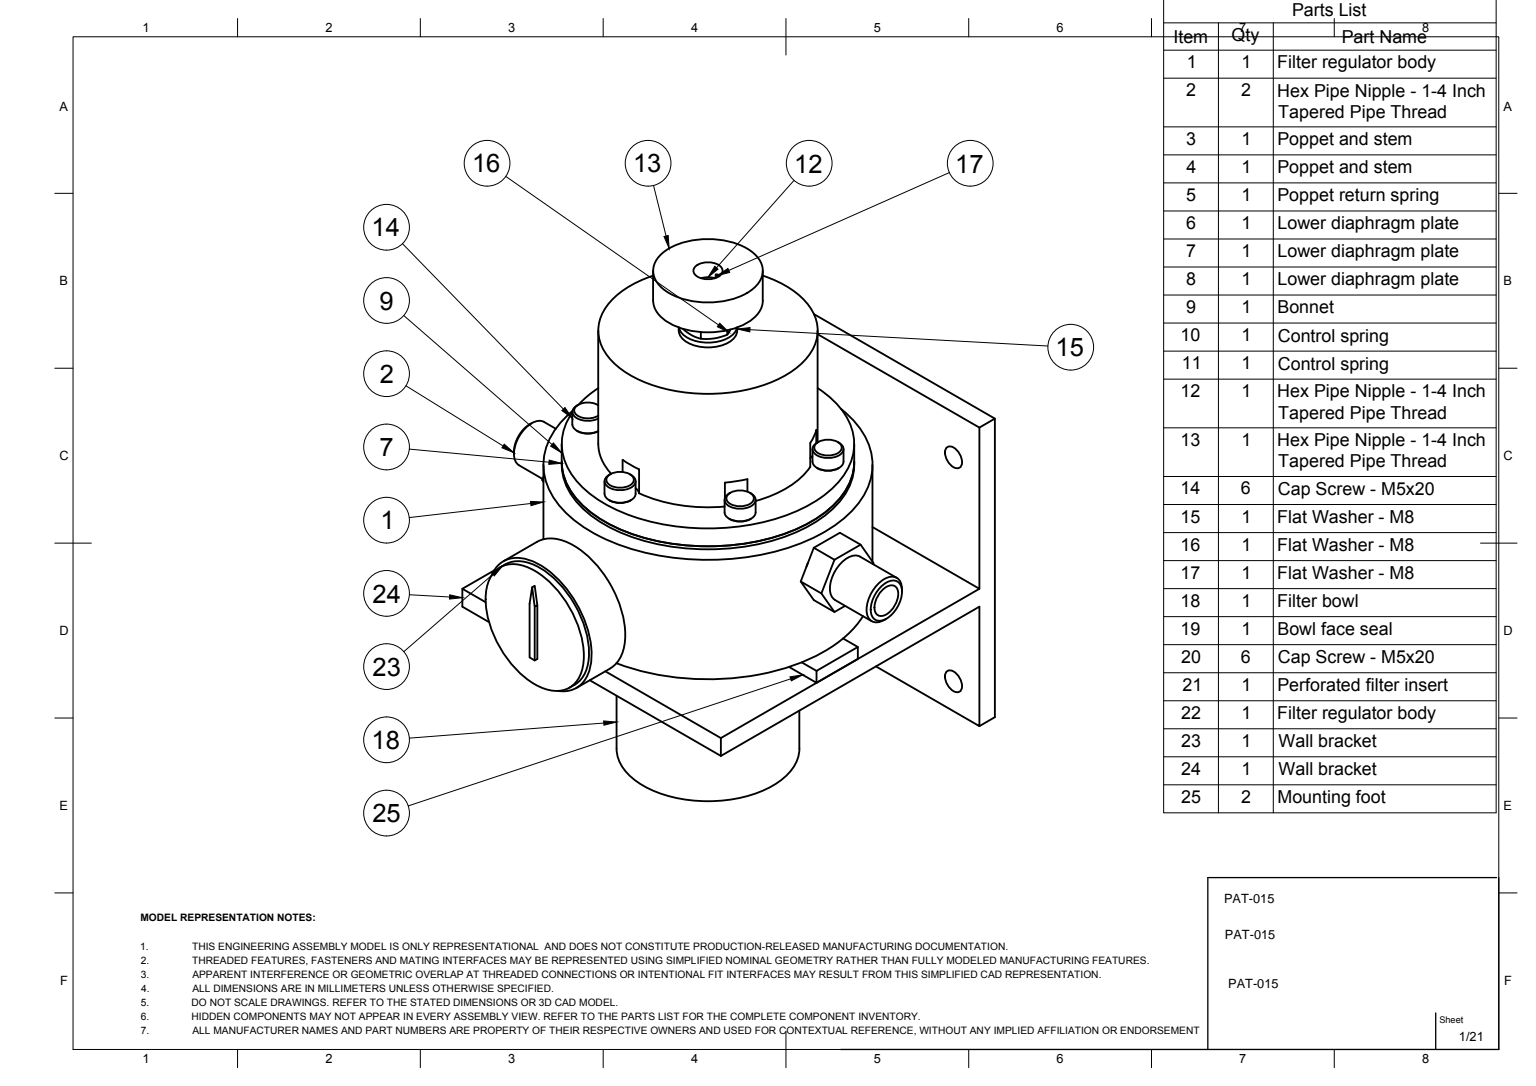
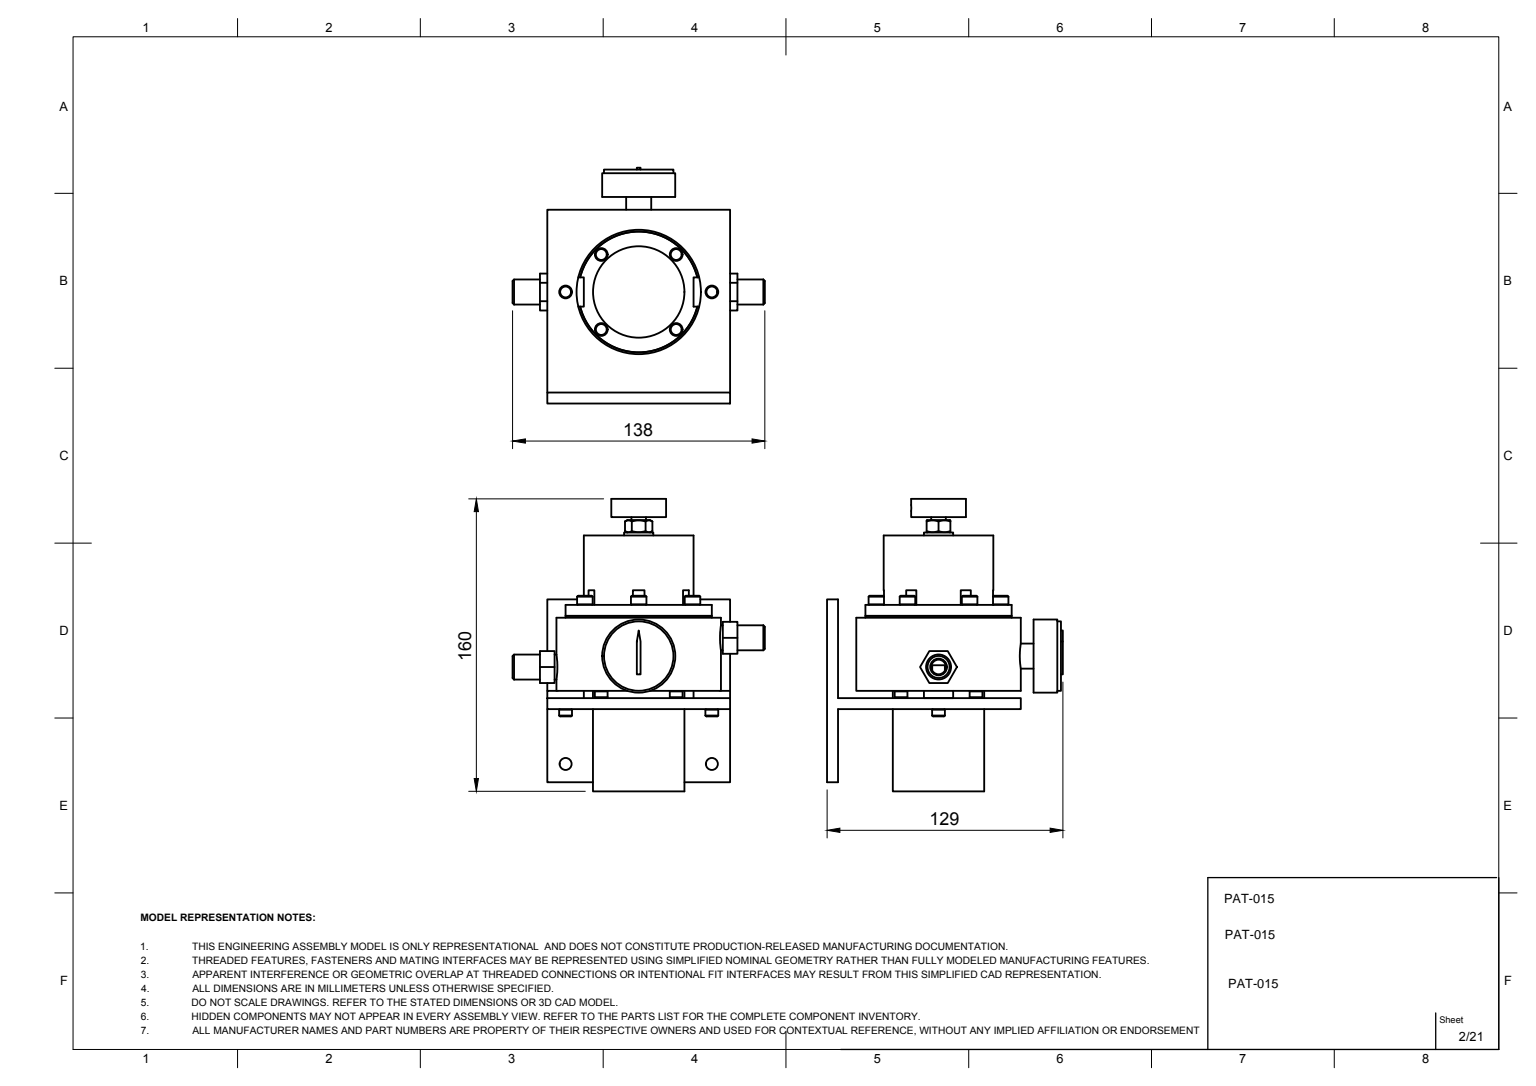
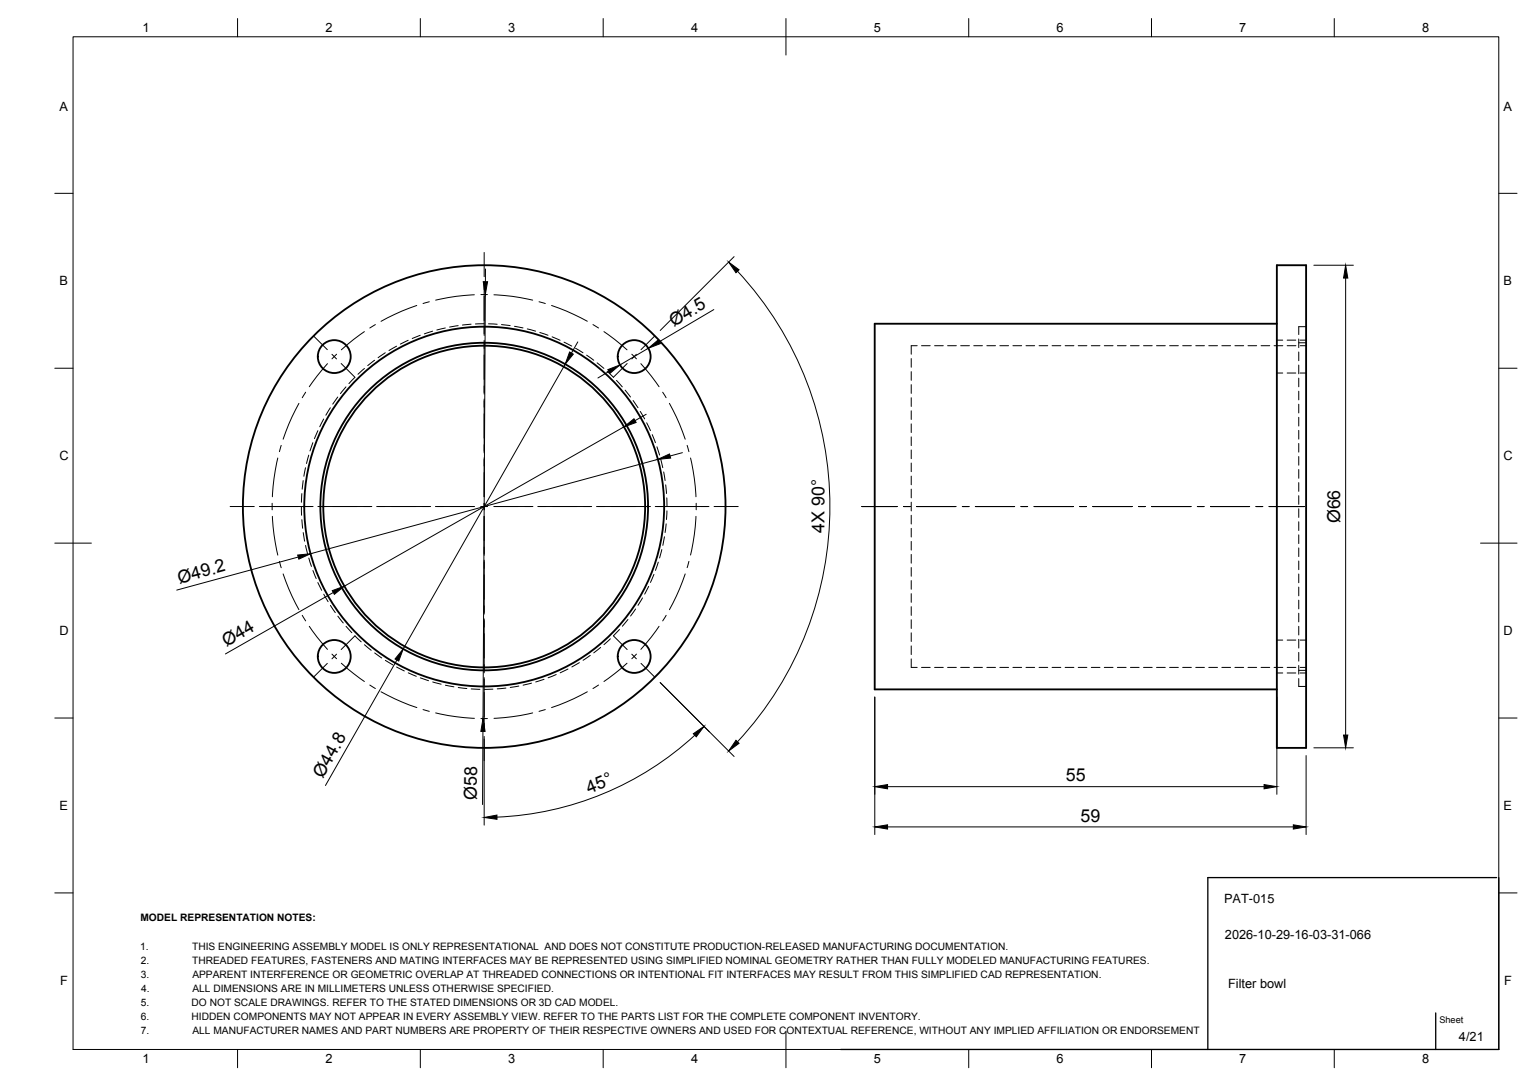
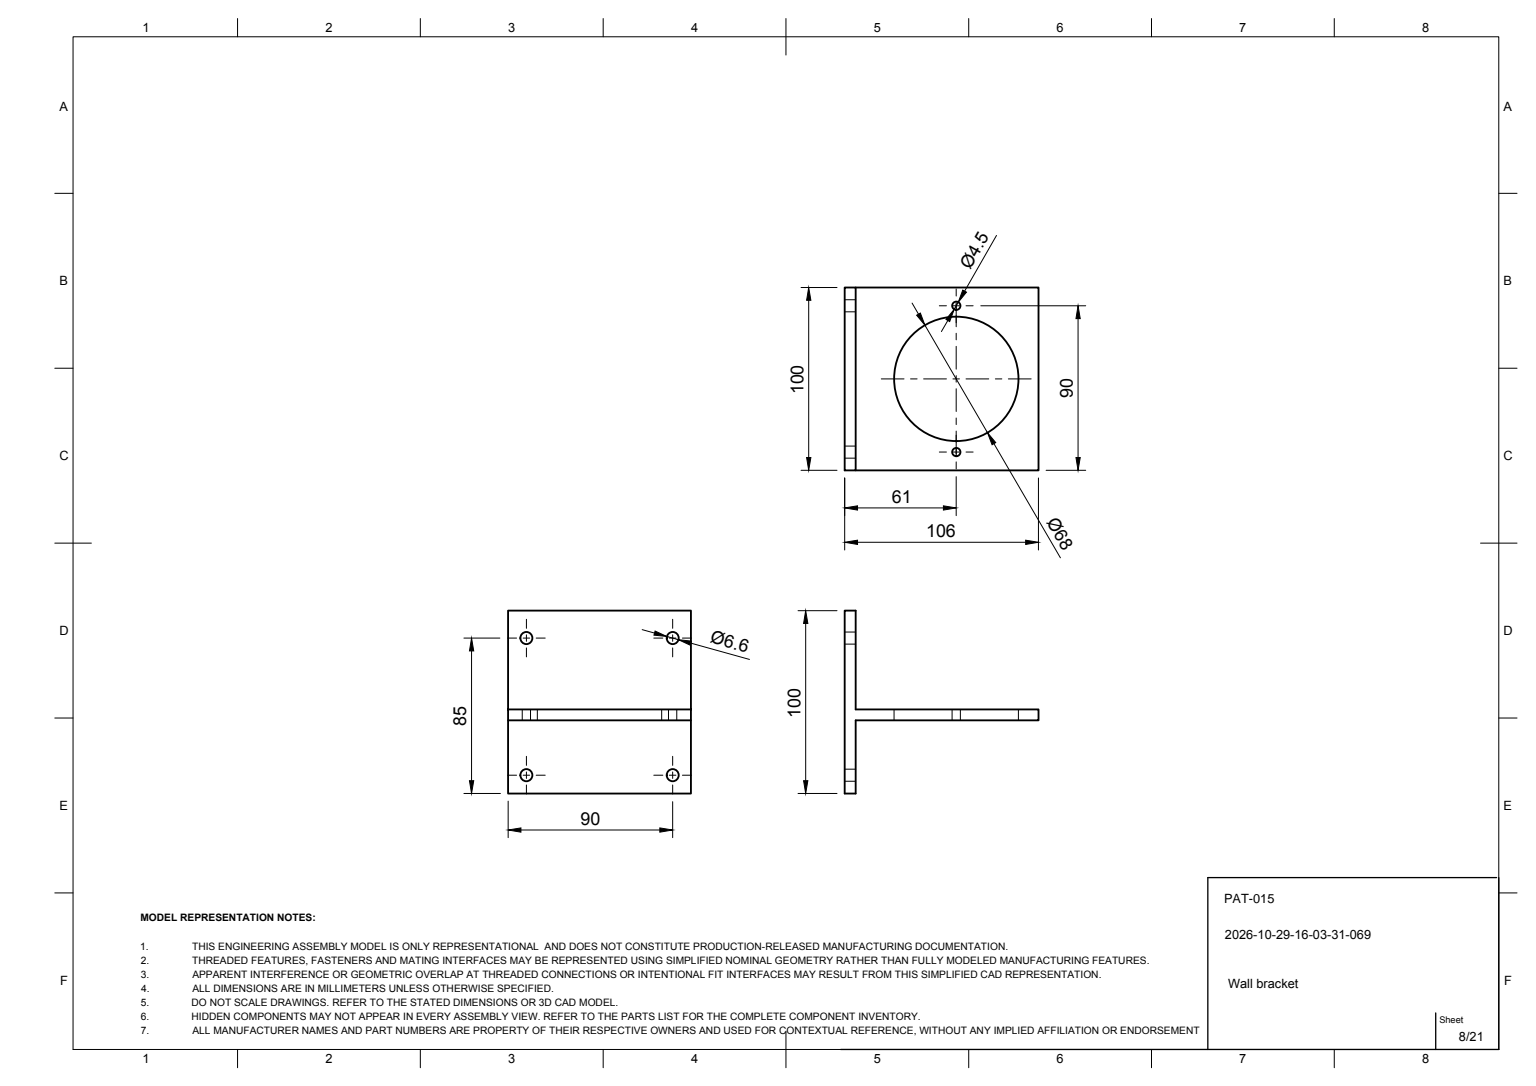
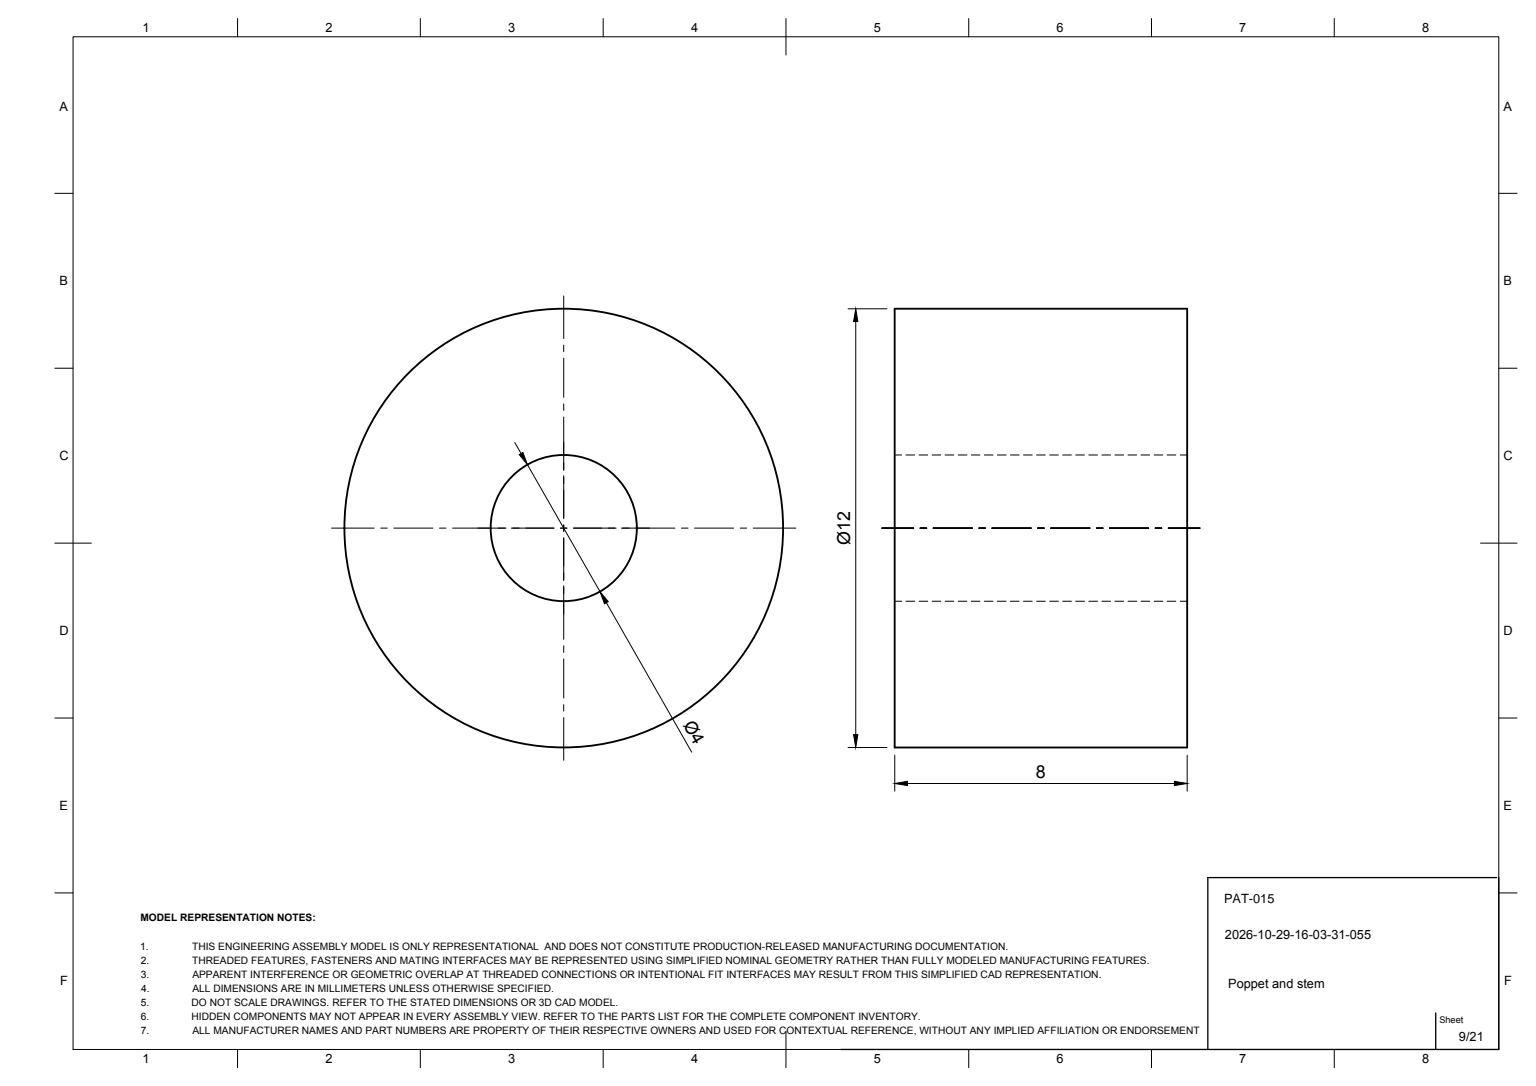
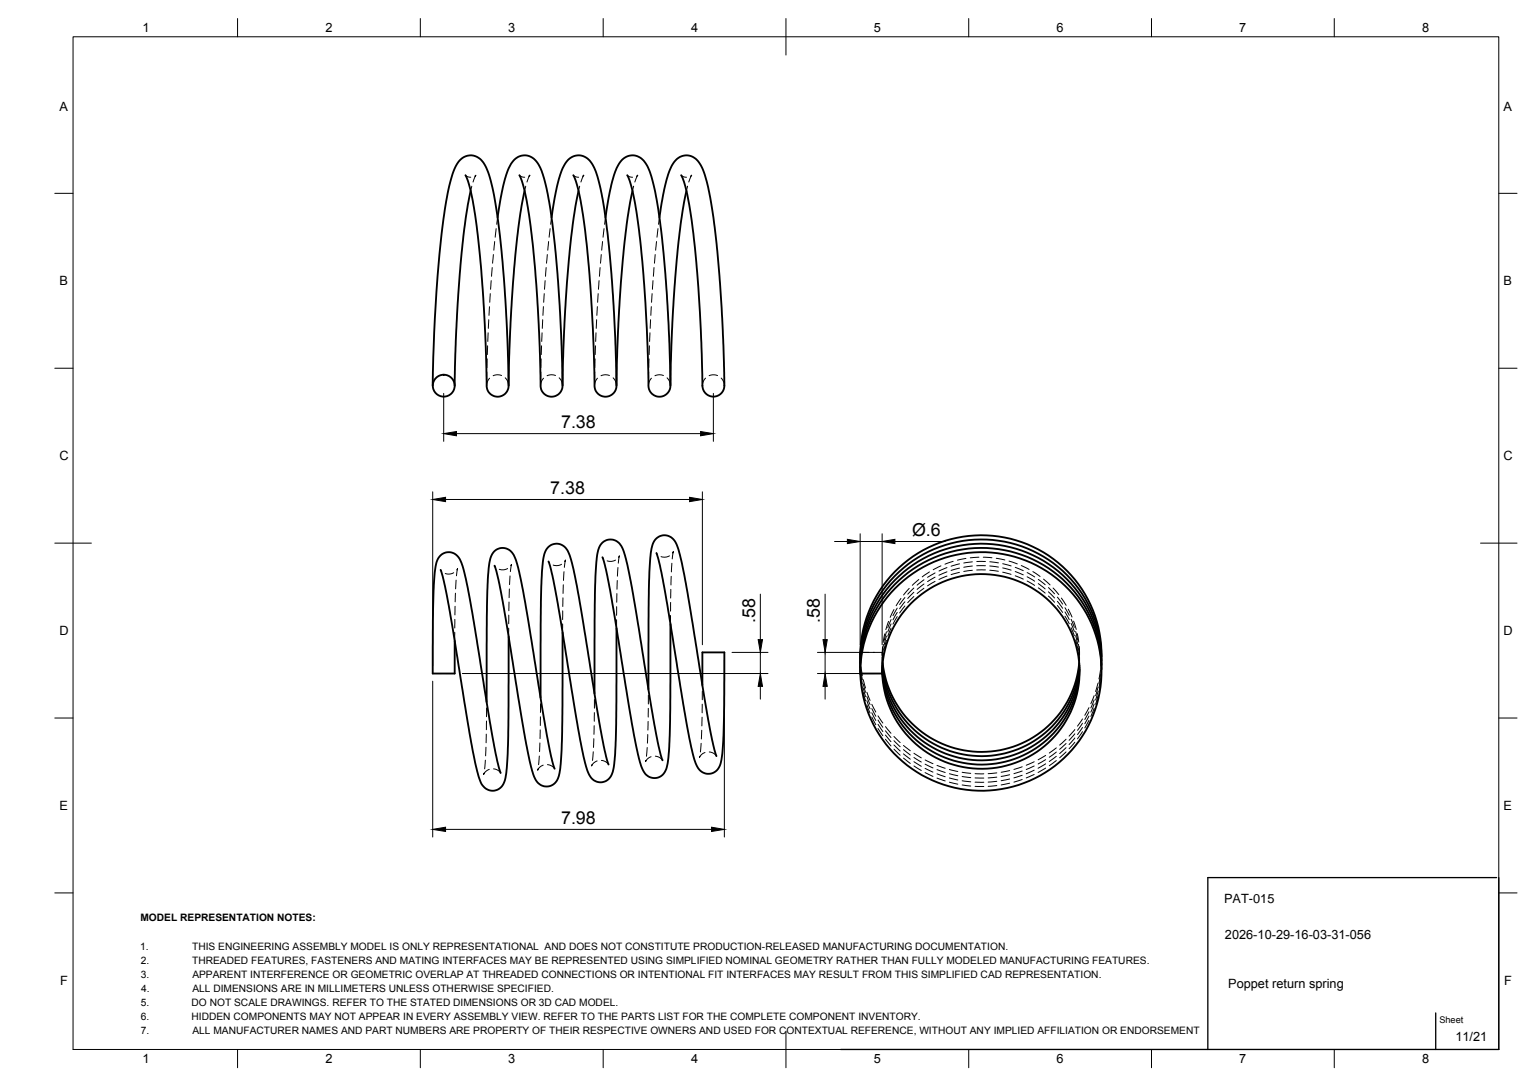
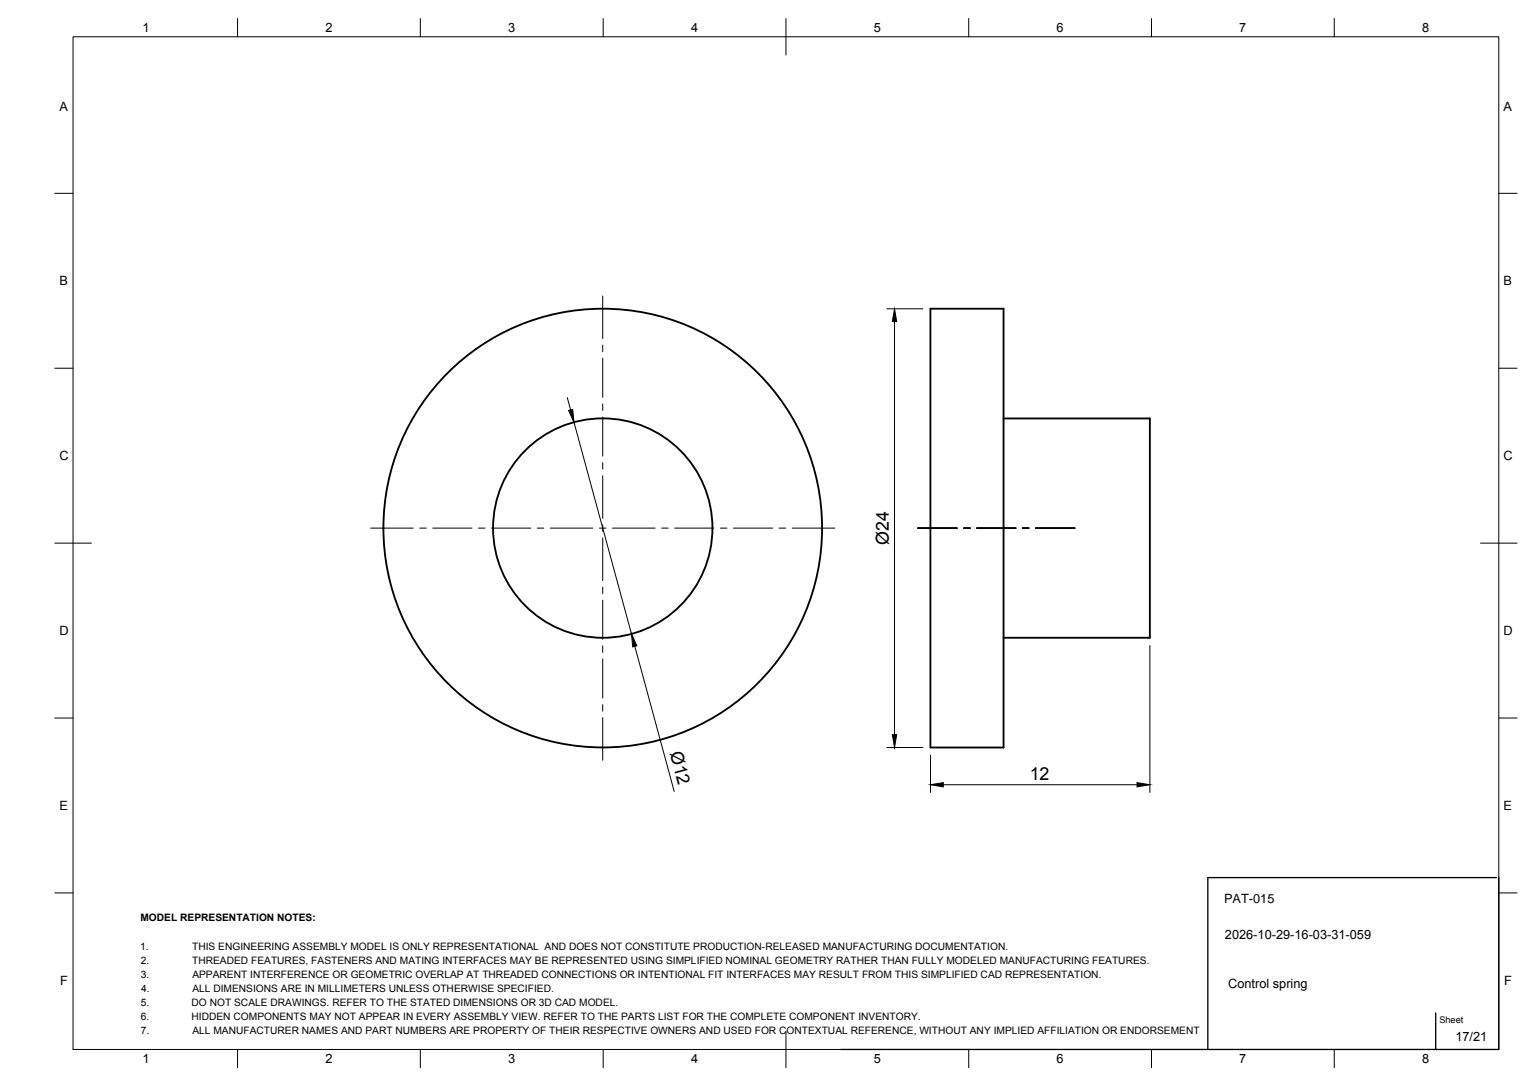
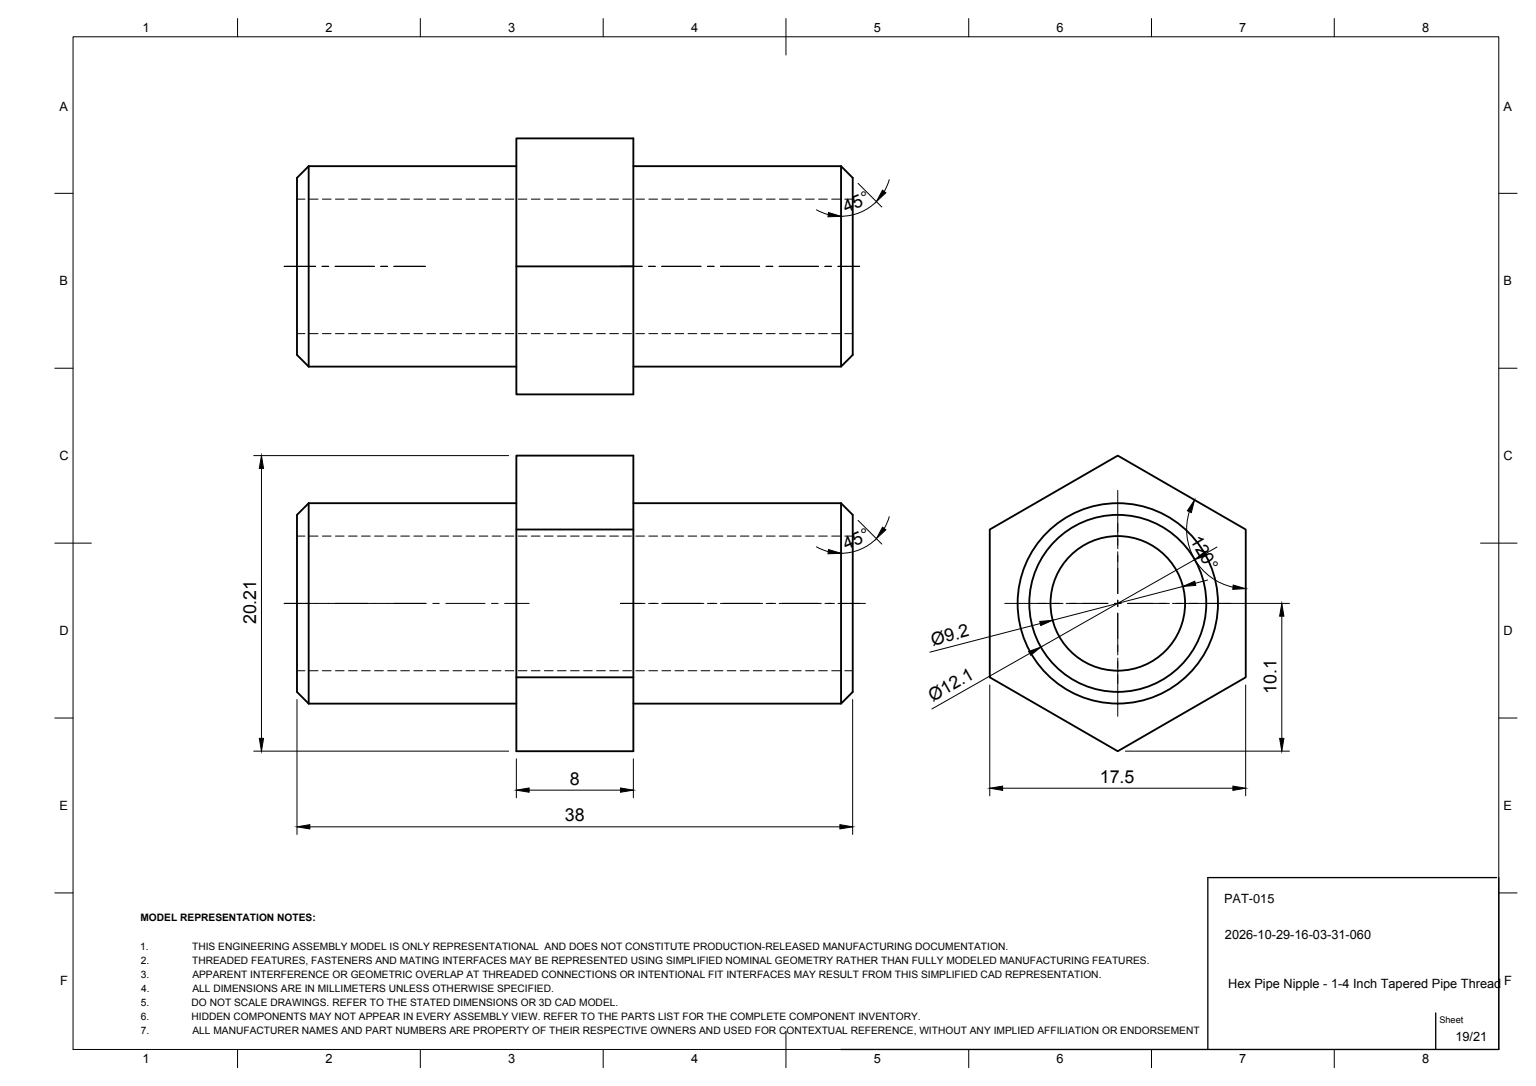
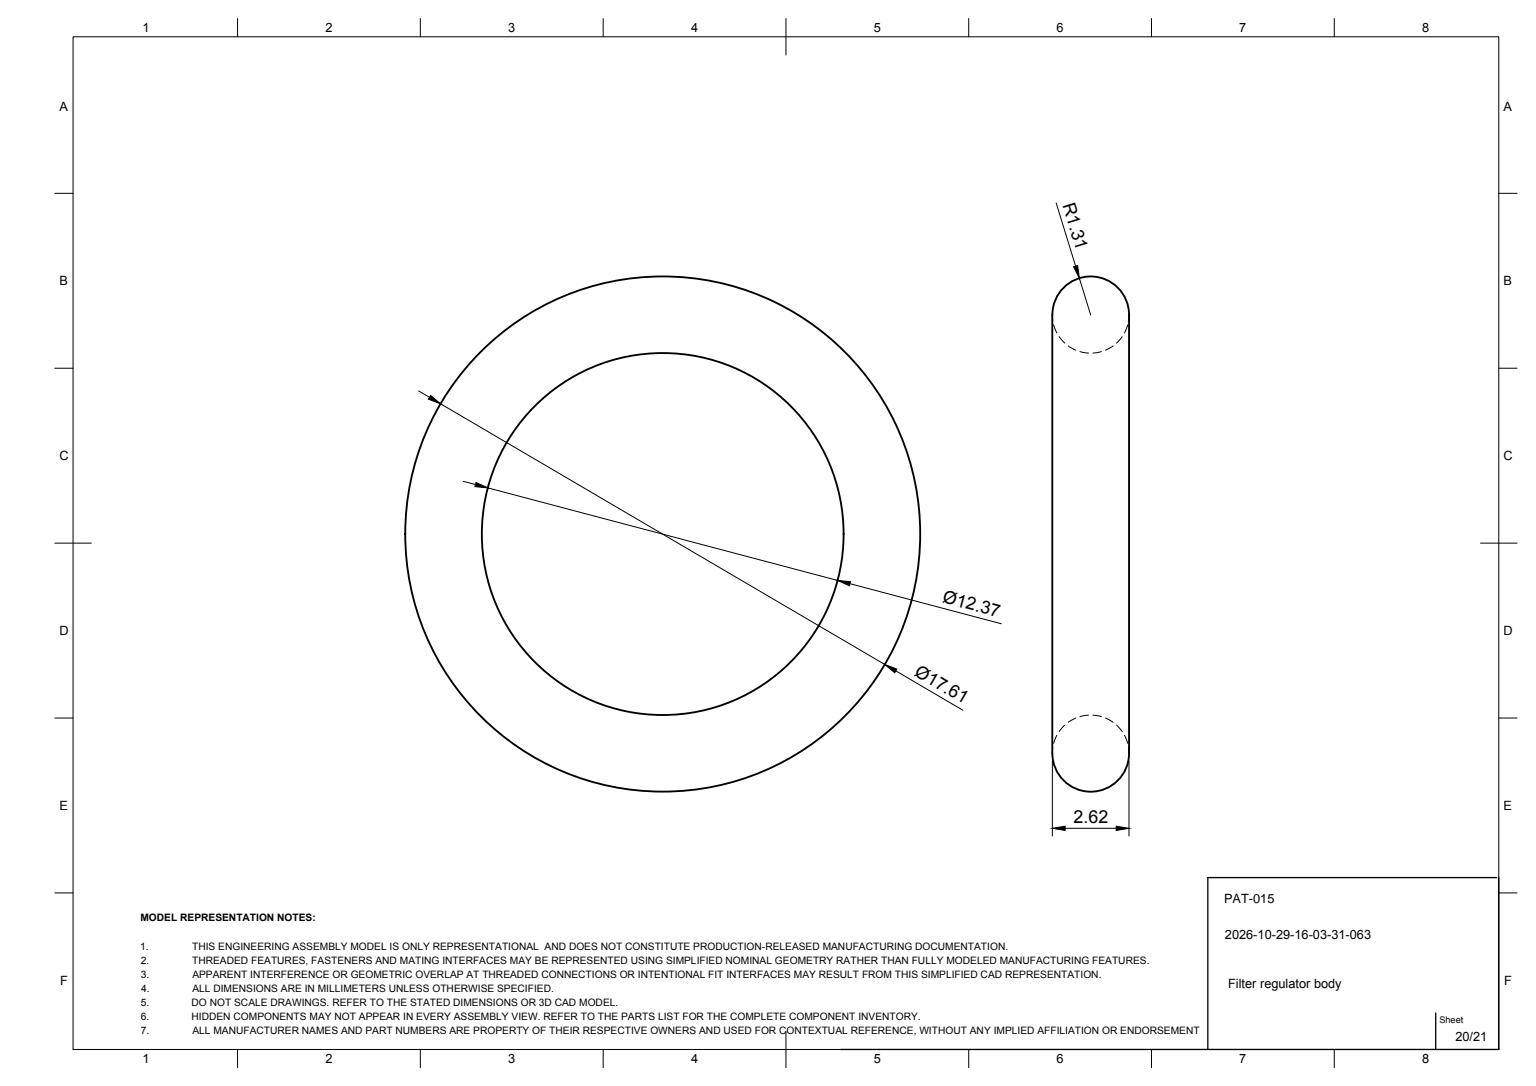
ISO-10303-21;
HEADER;
/* Generated by software containing ST-Developer
 * from STEP Tools, Inc. (www.steptools.com) 
 */

FILE_DESCRIPTION(
/* description */ ('PAT-015'),
/* implementation_level */ '2;1');

FILE_NAME(
/* name */ 'PAT-015',
/* time_stamp */ '2026-10-29T16:03:43-07:00',
/* author */ (''),
/* organization */ (''),
/* preprocessor_version */ 'ST-DEVELOPER v20.2',
/* originating_system */ 'Autodesk Translation Framework v15.17.0.0',
/* authorisation */ '');

FILE_SCHEMA (('AUTOMOTIVE_DESIGN { 1 0 10303 214 3 1 1 }'));
ENDSEC;

DATA;
#10=MECHANICAL_DESIGN_GEOMETRIC_PRESENTATION_REPRESENTATION('',(#230,#231,
#232,#233,#234,#235,#236,#237,#238,#239,#240,#241,#242,#243,#244,#245,#246,
#247,#248,#249,#250,#251,#252,#253,#254),#10266);
#11=ITEM_DEFINED_TRANSFORMATION($,$,#4971,#5521);
#12=ITEM_DEFINED_TRANSFORMATION($,$,#5114,#5522);
#13=ITEM_DEFINED_TRANSFORMATION($,$,#5118,#5523);
#14=ITEM_DEFINED_TRANSFORMATION($,$,#5144,#5524);
#15=ITEM_DEFINED_TRANSFORMATION($,$,#5166,#5525);
#16=ITEM_DEFINED_TRANSFORMATION($,$,#5198,#5526);
#17=ITEM_DEFINED_TRANSFORMATION($,$,#5198,#5527);
#18=ITEM_DEFINED_TRANSFORMATION($,$,#5222,#5528);
#19=ITEM_DEFINED_TRANSFORMATION($,$,#5231,#5529);
#20=ITEM_DEFINED_TRANSFORMATION($,$,#5253,#5530);
#21=ITEM_DEFINED_TRANSFORMATION($,$,#5262,#5531);
#22=ITEM_DEFINED_TRANSFORMATION($,$,#5289,#5532);
#23=ITEM_DEFINED_TRANSFORMATION($,$,#5306,#5533);
#24=ITEM_DEFINED_TRANSFORMATION($,$,#5377,#5534);
#25=ITEM_DEFINED_TRANSFORMATION($,$,#5382,#5535);
#26=ITEM_DEFINED_TRANSFORMATION($,$,#5392,#5536);
#27=ITEM_DEFINED_TRANSFORMATION($,$,#5398,#5537);
#28=ITEM_DEFINED_TRANSFORMATION($,$,#5413,#5538);
#29=ITEM_DEFINED_TRANSFORMATION($,$,#5413,#5539);
#30=ITEM_DEFINED_TRANSFORMATION($,$,#5413,#5540);
#31=ITEM_DEFINED_TRANSFORMATION($,$,#5413,#5541);
#32=ITEM_DEFINED_TRANSFORMATION($,$,#5413,#5542);
#33=ITEM_DEFINED_TRANSFORMATION($,$,#5413,#5543);
#34=ITEM_DEFINED_TRANSFORMATION($,$,#5439,#5544);
#35=ITEM_DEFINED_TRANSFORMATION($,$,#5448,#5545);
#36=ITEM_DEFINED_TRANSFORMATION($,$,#5464,#5546);
#37=ITEM_DEFINED_TRANSFORMATION($,$,#5495,#5547);
#38=ITEM_DEFINED_TRANSFORMATION($,$,#5495,#5548);
#39=ITEM_DEFINED_TRANSFORMATION($,$,#5495,#5549);
#40=ITEM_DEFINED_TRANSFORMATION($,$,#5495,#5550);
#41=ITEM_DEFINED_TRANSFORMATION($,$,#5481,#5551);
#42=ITEM_DEFINED_TRANSFORMATION($,$,#5485,#5552);
#43=ITEM_DEFINED_TRANSFORMATION($,$,#5495,#5553);
#44=ITEM_DEFINED_TRANSFORMATION($,$,#5485,#5554);
#45=ITEM_DEFINED_TRANSFORMATION($,$,#5495,#5555);
#46=(
REPRESENTATION_RELATIONSHIP($,$,#10355,#10354)
REPRESENTATION_RELATIONSHIP_WITH_TRANSFORMATION(#11)
SHAPE_REPRESENTATION_RELATIONSHIP()
);
#47=(
REPRESENTATION_RELATIONSHIP($,$,#10356,#10354)
REPRESENTATION_RELATIONSHIP_WITH_TRANSFORMATION(#12)
SHAPE_REPRESENTATION_RELATIONSHIP()
);
#48=(
REPRESENTATION_RELATIONSHIP($,$,#10357,#10354)
REPRESENTATION_RELATIONSHIP_WITH_TRANSFORMATION(#13)
SHAPE_REPRESENTATION_RELATIONSHIP()
);
#49=(
REPRESENTATION_RELATIONSHIP($,$,#10358,#10354)
REPRESENTATION_RELATIONSHIP_WITH_TRANSFORMATION(#14)
SHAPE_REPRESENTATION_RELATIONSHIP()
);
#50=(
REPRESENTATION_RELATIONSHIP($,$,#10359,#10354)
REPRESENTATION_RELATIONSHIP_WITH_TRANSFORMATION(#15)
SHAPE_REPRESENTATION_RELATIONSHIP()
);
#51=(
REPRESENTATION_RELATIONSHIP($,$,#10360,#10354)
REPRESENTATION_RELATIONSHIP_WITH_TRANSFORMATION(#16)
SHAPE_REPRESENTATION_RELATIONSHIP()
);
#52=(
REPRESENTATION_RELATIONSHIP($,$,#10360,#10354)
REPRESENTATION_RELATIONSHIP_WITH_TRANSFORMATION(#17)
SHAPE_REPRESENTATION_RELATIONSHIP()
);
#53=(
REPRESENTATION_RELATIONSHIP($,$,#10361,#10354)
REPRESENTATION_RELATIONSHIP_WITH_TRANSFORMATION(#18)
SHAPE_REPRESENTATION_RELATIONSHIP()
);
#54=(
REPRESENTATION_RELATIONSHIP($,$,#10362,#10354)
REPRESENTATION_RELATIONSHIP_WITH_TRANSFORMATION(#19)
SHAPE_REPRESENTATION_RELATIONSHIP()
);
#55=(
REPRESENTATION_RELATIONSHIP($,$,#10363,#10354)
REPRESENTATION_RELATIONSHIP_WITH_TRANSFORMATION(#20)
SHAPE_REPRESENTATION_RELATIONSHIP()
);
#56=(
REPRESENTATION_RELATIONSHIP($,$,#10364,#10354)
REPRESENTATION_RELATIONSHIP_WITH_TRANSFORMATION(#21)
SHAPE_REPRESENTATION_RELATIONSHIP()
);
#57=(
REPRESENTATION_RELATIONSHIP($,$,#10365,#10354)
REPRESENTATION_RELATIONSHIP_WITH_TRANSFORMATION(#22)
SHAPE_REPRESENTATION_RELATIONSHIP()
);
#58=(
REPRESENTATION_RELATIONSHIP($,$,#10366,#10354)
REPRESENTATION_RELATIONSHIP_WITH_TRANSFORMATION(#23)
SHAPE_REPRESENTATION_RELATIONSHIP()
);
#59=(
REPRESENTATION_RELATIONSHIP($,$,#10367,#10354)
REPRESENTATION_RELATIONSHIP_WITH_TRANSFORMATION(#24)
SHAPE_REPRESENTATION_RELATIONSHIP()
);
#60=(
REPRESENTATION_RELATIONSHIP($,$,#10368,#10354)
REPRESENTATION_RELATIONSHIP_WITH_TRANSFORMATION(#25)
SHAPE_REPRESENTATION_RELATIONSHIP()
);
#61=(
REPRESENTATION_RELATIONSHIP($,$,#10369,#10354)
REPRESENTATION_RELATIONSHIP_WITH_TRANSFORMATION(#26)
SHAPE_REPRESENTATION_RELATIONSHIP()
);
#62=(
REPRESENTATION_RELATIONSHIP($,$,#10370,#10354)
REPRESENTATION_RELATIONSHIP_WITH_TRANSFORMATION(#27)
SHAPE_REPRESENTATION_RELATIONSHIP()
);
#63=(
REPRESENTATION_RELATIONSHIP($,$,#10371,#10354)
REPRESENTATION_RELATIONSHIP_WITH_TRANSFORMATION(#28)
SHAPE_REPRESENTATION_RELATIONSHIP()
);
#64=(
REPRESENTATION_RELATIONSHIP($,$,#10371,#10354)
REPRESENTATION_RELATIONSHIP_WITH_TRANSFORMATION(#29)
SHAPE_REPRESENTATION_RELATIONSHIP()
);
#65=(
REPRESENTATION_RELATIONSHIP($,$,#10371,#10354)
REPRESENTATION_RELATIONSHIP_WITH_TRANSFORMATION(#30)
SHAPE_REPRESENTATION_RELATIONSHIP()
);
#66=(
REPRESENTATION_RELATIONSHIP($,$,#10371,#10354)
REPRESENTATION_RELATIONSHIP_WITH_TRANSFORMATION(#31)
SHAPE_REPRESENTATION_RELATIONSHIP()
);
#67=(
REPRESENTATION_RELATIONSHIP($,$,#10371,#10354)
REPRESENTATION_RELATIONSHIP_WITH_TRANSFORMATION(#32)
SHAPE_REPRESENTATION_RELATIONSHIP()
);
#68=(
REPRESENTATION_RELATIONSHIP($,$,#10371,#10354)
REPRESENTATION_RELATIONSHIP_WITH_TRANSFORMATION(#33)
SHAPE_REPRESENTATION_RELATIONSHIP()
);
#69=(
REPRESENTATION_RELATIONSHIP($,$,#10372,#10354)
REPRESENTATION_RELATIONSHIP_WITH_TRANSFORMATION(#34)
SHAPE_REPRESENTATION_RELATIONSHIP()
);
#70=(
REPRESENTATION_RELATIONSHIP($,$,#10373,#10354)
REPRESENTATION_RELATIONSHIP_WITH_TRANSFORMATION(#35)
SHAPE_REPRESENTATION_RELATIONSHIP()
);
#71=(
REPRESENTATION_RELATIONSHIP($,$,#10374,#10354)
REPRESENTATION_RELATIONSHIP_WITH_TRANSFORMATION(#36)
SHAPE_REPRESENTATION_RELATIONSHIP()
);
#72=(
REPRESENTATION_RELATIONSHIP($,$,#10377,#10354)
REPRESENTATION_RELATIONSHIP_WITH_TRANSFORMATION(#37)
SHAPE_REPRESENTATION_RELATIONSHIP()
);
#73=(
REPRESENTATION_RELATIONSHIP($,$,#10377,#10354)
REPRESENTATION_RELATIONSHIP_WITH_TRANSFORMATION(#38)
SHAPE_REPRESENTATION_RELATIONSHIP()
);
#74=(
REPRESENTATION_RELATIONSHIP($,$,#10377,#10354)
REPRESENTATION_RELATIONSHIP_WITH_TRANSFORMATION(#39)
SHAPE_REPRESENTATION_RELATIONSHIP()
);
#75=(
REPRESENTATION_RELATIONSHIP($,$,#10377,#10354)
REPRESENTATION_RELATIONSHIP_WITH_TRANSFORMATION(#40)
SHAPE_REPRESENTATION_RELATIONSHIP()
);
#76=(
REPRESENTATION_RELATIONSHIP($,$,#10375,#10354)
REPRESENTATION_RELATIONSHIP_WITH_TRANSFORMATION(#41)
SHAPE_REPRESENTATION_RELATIONSHIP()
);
#77=(
REPRESENTATION_RELATIONSHIP($,$,#10376,#10354)
REPRESENTATION_RELATIONSHIP_WITH_TRANSFORMATION(#42)
SHAPE_REPRESENTATION_RELATIONSHIP()
);
#78=(
REPRESENTATION_RELATIONSHIP($,$,#10377,#10354)
REPRESENTATION_RELATIONSHIP_WITH_TRANSFORMATION(#43)
SHAPE_REPRESENTATION_RELATIONSHIP()
);
#79=(
REPRESENTATION_RELATIONSHIP($,$,#10376,#10354)
REPRESENTATION_RELATIONSHIP_WITH_TRANSFORMATION(#44)
SHAPE_REPRESENTATION_RELATIONSHIP()
);
#80=(
REPRESENTATION_RELATIONSHIP($,$,#10377,#10354)
REPRESENTATION_RELATIONSHIP_WITH_TRANSFORMATION(#45)
SHAPE_REPRESENTATION_RELATIONSHIP()
);
#81=CONTEXT_DEPENDENT_SHAPE_REPRESENTATION(#46,#10319);
#82=CONTEXT_DEPENDENT_SHAPE_REPRESENTATION(#47,#10320);
#83=CONTEXT_DEPENDENT_SHAPE_REPRESENTATION(#48,#10321);
#84=CONTEXT_DEPENDENT_SHAPE_REPRESENTATION(#49,#10322);
#85=CONTEXT_DEPENDENT_SHAPE_REPRESENTATION(#50,#10323);
#86=CONTEXT_DEPENDENT_SHAPE_REPRESENTATION(#51,#10324);
#87=CONTEXT_DEPENDENT_SHAPE_REPRESENTATION(#52,#10325);
#88=CONTEXT_DEPENDENT_SHAPE_REPRESENTATION(#53,#10326);
#89=CONTEXT_DEPENDENT_SHAPE_REPRESENTATION(#54,#10327);
#90=CONTEXT_DEPENDENT_SHAPE_REPRESENTATION(#55,#10328);
#91=CONTEXT_DEPENDENT_SHAPE_REPRESENTATION(#56,#10329);
#92=CONTEXT_DEPENDENT_SHAPE_REPRESENTATION(#57,#10330);
#93=CONTEXT_DEPENDENT_SHAPE_REPRESENTATION(#58,#10331);
#94=CONTEXT_DEPENDENT_SHAPE_REPRESENTATION(#59,#10332);
#95=CONTEXT_DEPENDENT_SHAPE_REPRESENTATION(#60,#10333);
#96=CONTEXT_DEPENDENT_SHAPE_REPRESENTATION(#61,#10334);
#97=CONTEXT_DEPENDENT_SHAPE_REPRESENTATION(#62,#10335);
#98=CONTEXT_DEPENDENT_SHAPE_REPRESENTATION(#63,#10336);
#99=CONTEXT_DEPENDENT_SHAPE_REPRESENTATION(#64,#10337);
#100=CONTEXT_DEPENDENT_SHAPE_REPRESENTATION(#65,#10338);
#101=CONTEXT_DEPENDENT_SHAPE_REPRESENTATION(#66,#10339);
#102=CONTEXT_DEPENDENT_SHAPE_REPRESENTATION(#67,#10340);
#103=CONTEXT_DEPENDENT_SHAPE_REPRESENTATION(#68,#10341);
#104=CONTEXT_DEPENDENT_SHAPE_REPRESENTATION(#69,#10342);
#105=CONTEXT_DEPENDENT_SHAPE_REPRESENTATION(#70,#10343);
#106=CONTEXT_DEPENDENT_SHAPE_REPRESENTATION(#71,#10344);
#107=CONTEXT_DEPENDENT_SHAPE_REPRESENTATION(#72,#10345);
#108=CONTEXT_DEPENDENT_SHAPE_REPRESENTATION(#73,#10346);
#109=CONTEXT_DEPENDENT_SHAPE_REPRESENTATION(#74,#10347);
#110=CONTEXT_DEPENDENT_SHAPE_REPRESENTATION(#75,#10348);
#111=CONTEXT_DEPENDENT_SHAPE_REPRESENTATION(#76,#10349);
#112=CONTEXT_DEPENDENT_SHAPE_REPRESENTATION(#77,#10350);
#113=CONTEXT_DEPENDENT_SHAPE_REPRESENTATION(#78,#10351);
#114=CONTEXT_DEPENDENT_SHAPE_REPRESENTATION(#79,#10352);
#115=CONTEXT_DEPENDENT_SHAPE_REPRESENTATION(#80,#10353);
#116=NEXT_ASSEMBLY_USAGE_OCCURRENCE('Filter regulator body:1',
'Filter regulator body:1','Filter regulator body:1',#10379,#10380,
'Filter regulator body:1');
#117=NEXT_ASSEMBLY_USAGE_OCCURRENCE('Bowl face seal:1',
'Bowl face seal:1','Bowl face seal:1',#10379,#10381,'Bowl face seal:1');
#118=NEXT_ASSEMBLY_USAGE_OCCURRENCE('Perforated filter insert:1',
'Perforated filter insert:1','Perforated filter insert:1',#10379,#10382,
'Perforated filter insert:1');
#119=NEXT_ASSEMBLY_USAGE_OCCURRENCE('Gauge dummy:1','Gauge dummy:1',
'Gauge dummy:1',#10379,#10383,'Gauge dummy:1');
#120=NEXT_ASSEMBLY_USAGE_OCCURRENCE('Wall bracket:1','Wall bracket:1',
'Wall bracket:1',#10379,#10384,'Wall bracket:1');
#121=NEXT_ASSEMBLY_USAGE_OCCURRENCE(
'Hex Pipe Nipple - 1-4 Inch Tapered Pipe Thread:1',
'Hex Pipe Nipple - 1-4 Inch Tapered Pipe Thread:1',
'Hex Pipe Nipple - 1-4 Inch Tapered Pipe Thread:1',#10379,#10385,
'Hex Pipe Nipple - 1-4 Inch Tapered Pipe Thread:1');
#122=NEXT_ASSEMBLY_USAGE_OCCURRENCE(
'Hex Pipe Nipple - 1-4 Inch Tapered Pipe Thread:2',
'Hex Pipe Nipple - 1-4 Inch Tapered Pipe Thread:2',
'Hex Pipe Nipple - 1-4 Inch Tapered Pipe Thread:2',#10379,#10385,
'Hex Pipe Nipple - 1-4 Inch Tapered Pipe Thread:2');
#123=NEXT_ASSEMBLY_USAGE_OCCURRENCE('Valve seat:1','Valve seat:1',
'Valve seat:1',#10379,#10386,'Valve seat:1');
#124=NEXT_ASSEMBLY_USAGE_OCCURRENCE('Poppet and stem:1',
'Poppet and stem:1','Poppet and stem:1',#10379,#10387,
'Poppet and stem:1');
#125=NEXT_ASSEMBLY_USAGE_OCCURRENCE('Lower diaphragm plate:1',
'Lower diaphragm plate:1','Lower diaphragm plate:1',#10379,#10388,
'Lower diaphragm plate:1');
#126=NEXT_ASSEMBLY_USAGE_OCCURRENCE('Diaphragm:1','Diaphragm:1',
'Diaphragm:1',#10379,#10389,'Diaphragm:1');
#127=NEXT_ASSEMBLY_USAGE_OCCURRENCE('Upper diaphragm plate:1',
'Upper diaphragm plate:1','Upper diaphragm plate:1',#10379,#10390,
'Upper diaphragm plate:1');
#128=NEXT_ASSEMBLY_USAGE_OCCURRENCE('Bonnet:1','Bonnet:1','Bonnet:1',#10379,
#10391,'Bonnet:1');
#129=NEXT_ASSEMBLY_USAGE_OCCURRENCE('Control spring:1',
'Control spring:1','Control spring:1',#10379,#10392,'Control spring:1');
#130=NEXT_ASSEMBLY_USAGE_OCCURRENCE('Adjuster spring shoe:1',
'Adjuster spring shoe:1','Adjuster spring shoe:1',#10379,#10393,
'Adjuster spring shoe:1');
#131=NEXT_ASSEMBLY_USAGE_OCCURRENCE('Adjusting screw:1',
'Adjusting screw:1','Adjusting screw:1',#10379,#10394,
'Adjusting screw:1');
#132=NEXT_ASSEMBLY_USAGE_OCCURRENCE('Adjuster knob:1','Adjuster knob:1',
'Adjuster knob:1',#10379,#10395,'Adjuster knob:1');
#133=NEXT_ASSEMBLY_USAGE_OCCURRENCE('Cap Screw - M5x20:1',
'Cap Screw - M5x20:1','Cap Screw - M5x20:1',#10379,#10396,
'Cap Screw - M5x20:1');
#134=NEXT_ASSEMBLY_USAGE_OCCURRENCE('Cap Screw - M5x20:2',
'Cap Screw - M5x20:2','Cap Screw - M5x20:2',#10379,#10396,
'Cap Screw - M5x20:2');
#135=NEXT_ASSEMBLY_USAGE_OCCURRENCE('Cap Screw - M5x20:3',
'Cap Screw - M5x20:3','Cap Screw - M5x20:3',#10379,#10396,
'Cap Screw - M5x20:3');
#136=NEXT_ASSEMBLY_USAGE_OCCURRENCE('Cap Screw - M5x20:4',
'Cap Screw - M5x20:4','Cap Screw - M5x20:4',#10379,#10396,
'Cap Screw - M5x20:4');
#137=NEXT_ASSEMBLY_USAGE_OCCURRENCE('Cap Screw - M5x20:5',
'Cap Screw - M5x20:5','Cap Screw - M5x20:5',#10379,#10396,
'Cap Screw - M5x20:5');
#138=NEXT_ASSEMBLY_USAGE_OCCURRENCE('Cap Screw - M5x20:6',
'Cap Screw - M5x20:6','Cap Screw - M5x20:6',#10379,#10396,
'Cap Screw - M5x20:6');
#139=NEXT_ASSEMBLY_USAGE_OCCURRENCE('Flat Washer - M8:1',
'Flat Washer - M8:1','Flat Washer - M8:1',#10379,#10397,
'Flat Washer - M8:1');
#140=NEXT_ASSEMBLY_USAGE_OCCURRENCE('Hex Nut - M8:1','Hex Nut - M8:1',
'Hex Nut - M8:1',#10379,#10398,'Hex Nut - M8:1');
#141=NEXT_ASSEMBLY_USAGE_OCCURRENCE('Socket Set Screw - M4x6:1',
'Socket Set Screw - M4x6:1','Socket Set Screw - M4x6:1',#10379,#10399,
'Socket Set Screw - M4x6:1');
#142=NEXT_ASSEMBLY_USAGE_OCCURRENCE('Cap Screw - M4x16:1',
'Cap Screw - M4x16:1','Cap Screw - M4x16:1',#10379,#10402,
'Cap Screw - M4x16:1');
#143=NEXT_ASSEMBLY_USAGE_OCCURRENCE('Cap Screw - M4x16:2',
'Cap Screw - M4x16:2','Cap Screw - M4x16:2',#10379,#10402,
'Cap Screw - M4x16:2');
#144=NEXT_ASSEMBLY_USAGE_OCCURRENCE('Cap Screw - M4x16:3',
'Cap Screw - M4x16:3','Cap Screw - M4x16:3',#10379,#10402,
'Cap Screw - M4x16:3');
#145=NEXT_ASSEMBLY_USAGE_OCCURRENCE('Cap Screw - M4x16:4',
'Cap Screw - M4x16:4','Cap Screw - M4x16:4',#10379,#10402,
'Cap Screw - M4x16:4');
#146=NEXT_ASSEMBLY_USAGE_OCCURRENCE('O-Ring:1','O-Ring:1','O-Ring:1',#10379,
#10400,'O-Ring:1');
#147=NEXT_ASSEMBLY_USAGE_OCCURRENCE('Mounting foot:1','Mounting foot:1',
'Mounting foot:1',#10379,#10401,'Mounting foot:1');
#148=NEXT_ASSEMBLY_USAGE_OCCURRENCE('Cap Screw - M4x16:5',
'Cap Screw - M4x16:5','Cap Screw - M4x16:5',#10379,#10402,
'Cap Screw - M4x16:5');
#149=NEXT_ASSEMBLY_USAGE_OCCURRENCE('Mounting foot:2','Mounting foot:2',
'Mounting foot:2',#10379,#10401,'Mounting foot:2');
#150=NEXT_ASSEMBLY_USAGE_OCCURRENCE('Cap Screw - M4x16:6',
'Cap Screw - M4x16:6','Cap Screw - M4x16:6',#10379,#10402,
'Cap Screw - M4x16:6');
#151=(
BOUNDED_CURVE()
B_SPLINE_CURVE(2,(#9947,#9948,#9949),.UNSPECIFIED.,.F.,.F.)
B_SPLINE_CURVE_WITH_KNOTS((3,3),(0.14973948338295,0.97160236658079),
 .UNSPECIFIED.)
CURVE()
GEOMETRIC_REPRESENTATION_ITEM()
RATIONAL_B_SPLINE_CURVE((1.07140024848292,1.23714644374248,1.07140024848292))
REPRESENTATION_ITEM('')
);
#152=(
BOUNDED_CURVE()
B_SPLINE_CURVE(2,(#9951,#9952,#9953),.UNSPECIFIED.,.F.,.F.)
B_SPLINE_CURVE_WITH_KNOTS((3,3),(0.14973948338295,0.971602366580789),
 .UNSPECIFIED.)
CURVE()
GEOMETRIC_REPRESENTATION_ITEM()
RATIONAL_B_SPLINE_CURVE((1.07140024848292,1.23714644374248,1.07140024848292))
REPRESENTATION_ITEM('')
);
#153=(
BOUNDED_CURVE()
B_SPLINE_CURVE(2,(#9958,#9959,#9960),.UNSPECIFIED.,.F.,.F.)
B_SPLINE_CURVE_WITH_KNOTS((3,3),(0.14973948338295,0.97160236658079),
 .UNSPECIFIED.)
CURVE()
GEOMETRIC_REPRESENTATION_ITEM()
RATIONAL_B_SPLINE_CURVE((1.07140024848292,1.23714644374248,1.07140024848292))
REPRESENTATION_ITEM('')
);
#154=(
BOUNDED_CURVE()
B_SPLINE_CURVE(2,(#9962,#9963,#9964),.UNSPECIFIED.,.F.,.F.)
B_SPLINE_CURVE_WITH_KNOTS((3,3),(0.14973948338295,0.97160236658079),
 .UNSPECIFIED.)
CURVE()
GEOMETRIC_REPRESENTATION_ITEM()
RATIONAL_B_SPLINE_CURVE((1.07140024848292,1.23714644374248,1.07140024848292))
REPRESENTATION_ITEM('')
);
#155=(
BOUNDED_CURVE()
B_SPLINE_CURVE(2,(#9966,#9967,#9968),.UNSPECIFIED.,.F.,.F.)
B_SPLINE_CURVE_WITH_KNOTS((3,3),(0.14973948338295,0.971602366580789),
 .UNSPECIFIED.)
CURVE()
GEOMETRIC_REPRESENTATION_ITEM()
RATIONAL_B_SPLINE_CURVE((1.07140024848292,1.23714644374248,1.07140024848292))
REPRESENTATION_ITEM('')
);
#156=(
BOUNDED_CURVE()
B_SPLINE_CURVE(2,(#9969,#9970,#9971),.UNSPECIFIED.,.F.,.F.)
B_SPLINE_CURVE_WITH_KNOTS((3,3),(0.14973948338295,0.97160236658079),
 .UNSPECIFIED.)
CURVE()
GEOMETRIC_REPRESENTATION_ITEM()
RATIONAL_B_SPLINE_CURVE((1.07140024848292,1.23714644374248,1.07140024848292))
REPRESENTATION_ITEM('')
);
#157=(
BOUNDED_CURVE()
B_SPLINE_CURVE(2,(#9978,#9979,#9980),.UNSPECIFIED.,.F.,.F.)
B_SPLINE_CURVE_WITH_KNOTS((3,3),(0.14973948338295,0.97160236658079),
 .UNSPECIFIED.)
CURVE()
GEOMETRIC_REPRESENTATION_ITEM()
RATIONAL_B_SPLINE_CURVE((1.07140024848292,1.23714644374248,1.07140024848292))
REPRESENTATION_ITEM('')
);
#158=(
BOUNDED_CURVE()
B_SPLINE_CURVE(2,(#9982,#9983,#9984),.UNSPECIFIED.,.F.,.F.)
B_SPLINE_CURVE_WITH_KNOTS((3,3),(0.14973948338295,0.97160236658079),
 .UNSPECIFIED.)
CURVE()
GEOMETRIC_REPRESENTATION_ITEM()
RATIONAL_B_SPLINE_CURVE((1.07140024848292,1.23714644374248,1.07140024848292))
REPRESENTATION_ITEM('')
);
#159=(
BOUNDED_CURVE()
B_SPLINE_CURVE(2,(#9986,#9987,#9988),.UNSPECIFIED.,.F.,.F.)
B_SPLINE_CURVE_WITH_KNOTS((3,3),(0.14973948338295,0.971602366580789),
 .UNSPECIFIED.)
CURVE()
GEOMETRIC_REPRESENTATION_ITEM()
RATIONAL_B_SPLINE_CURVE((1.07140024848292,1.23714644374248,1.07140024848292))
REPRESENTATION_ITEM('')
);
#160=(
BOUNDED_CURVE()
B_SPLINE_CURVE(2,(#9990,#9991,#9992),.UNSPECIFIED.,.F.,.F.)
B_SPLINE_CURVE_WITH_KNOTS((3,3),(0.14973948338295,0.97160236658079),
 .UNSPECIFIED.)
CURVE()
GEOMETRIC_REPRESENTATION_ITEM()
RATIONAL_B_SPLINE_CURVE((1.07140024848292,1.23714644374248,1.07140024848292))
REPRESENTATION_ITEM('')
);
#161=(
BOUNDED_CURVE()
B_SPLINE_CURVE(2,(#9994,#9995,#9996),.UNSPECIFIED.,.F.,.F.)
B_SPLINE_CURVE_WITH_KNOTS((3,3),(0.14973948338295,0.97160236658079),
 .UNSPECIFIED.)
CURVE()
GEOMETRIC_REPRESENTATION_ITEM()
RATIONAL_B_SPLINE_CURVE((1.07140024848292,1.23714644374248,1.07140024848292))
REPRESENTATION_ITEM('')
);
#162=(
BOUNDED_CURVE()
B_SPLINE_CURVE(2,(#9997,#9998,#9999),.UNSPECIFIED.,.F.,.F.)
B_SPLINE_CURVE_WITH_KNOTS((3,3),(0.14973948338295,0.971602366580789),
 .UNSPECIFIED.)
CURVE()
GEOMETRIC_REPRESENTATION_ITEM()
RATIONAL_B_SPLINE_CURVE((1.07140024848292,1.23714644374248,1.07140024848292))
REPRESENTATION_ITEM('')
);
#163=ORIENTED_CLOSED_SHELL('',*,#4708,.F.);
#164=ORIENTED_CLOSED_SHELL('',*,#4715,.F.);
#165=BREP_WITH_VOIDS('Body1',#4707,(#163));
#166=BREP_WITH_VOIDS('Body1',#4714,(#164));
#167=B_SPLINE_SURFACE_WITH_KNOTS('',3,3,((#8962,#8963,#8964,#8965,#8966,
#8967,#8968,#8969,#8970,#8971,#8972,#8973,#8974,#8975,#8976,#8977,#8978,
#8979,#8980,#8981,#8982,#8983,#8984,#8985,#8986,#8987,#8988,#8989,#8990,
#8991,#8992,#8993,#8994,#8995,#8996,#8997,#8998,#8999,#9000,#9001,#9002,
#9003,#9004,#9005,#9006,#9007,#9008,#9009,#9010,#9011,#9012,#9013,#9014,
#9015,#9016,#9017,#9018,#9019,#9020,#9021,#9022,#9023,#9024,#9025,#9026,
#9027,#9028,#9029,#9030,#9031,#9032),(#9033,#9034,#9035,#9036,#9037,#9038,
#9039,#9040,#9041,#9042,#9043,#9044,#9045,#9046,#9047,#9048,#9049,#9050,
#9051,#9052,#9053,#9054,#9055,#9056,#9057,#9058,#9059,#9060,#9061,#9062,
#9063,#9064,#9065,#9066,#9067,#9068,#9069,#9070,#9071,#9072,#9073,#9074,
#9075,#9076,#9077,#9078,#9079,#9080,#9081,#9082,#9083,#9084,#9085,#9086,
#9087,#9088,#9089,#9090,#9091,#9092,#9093,#9094,#9095,#9096,#9097,#9098,
#9099,#9100,#9101,#9102,#9103),(#9104,#9105,#9106,#9107,#9108,#9109,#9110,
#9111,#9112,#9113,#9114,#9115,#9116,#9117,#9118,#9119,#9120,#9121,#9122,
#9123,#9124,#9125,#9126,#9127,#9128,#9129,#9130,#9131,#9132,#9133,#9134,
#9135,#9136,#9137,#9138,#9139,#9140,#9141,#9142,#9143,#9144,#9145,#9146,
#9147,#9148,#9149,#9150,#9151,#9152,#9153,#9154,#9155,#9156,#9157,#9158,
#9159,#9160,#9161,#9162,#9163,#9164,#9165,#9166,#9167,#9168,#9169,#9170,
#9171,#9172,#9173,#9174),(#9175,#9176,#9177,#9178,#9179,#9180,#9181,#9182,
#9183,#9184,#9185,#9186,#9187,#9188,#9189,#9190,#9191,#9192,#9193,#9194,
#9195,#9196,#9197,#9198,#9199,#9200,#9201,#9202,#9203,#9204,#9205,#9206,
#9207,#9208,#9209,#9210,#9211,#9212,#9213,#9214,#9215,#9216,#9217,#9218,
#9219,#9220,#9221,#9222,#9223,#9224,#9225,#9226,#9227,#9228,#9229,#9230,
#9231,#9232,#9233,#9234,#9235,#9236,#9237,#9238,#9239,#9240,#9241,#9242,
#9243,#9244,#9245),(#9246,#9247,#9248,#9249,#9250,#9251,#9252,#9253,#9254,
#9255,#9256,#9257,#9258,#9259,#9260,#9261,#9262,#9263,#9264,#9265,#9266,
#9267,#9268,#9269,#9270,#9271,#9272,#9273,#9274,#9275,#9276,#9277,#9278,
#9279,#9280,#9281,#9282,#9283,#9284,#9285,#9286,#9287,#9288,#9289,#9290,
#9291,#9292,#9293,#9294,#9295,#9296,#9297,#9298,#9299,#9300,#9301,#9302,
#9303,#9304,#9305,#9306,#9307,#9308,#9309,#9310,#9311,#9312,#9313,#9314,
#9315,#9316),(#9317,#9318,#9319,#9320,#9321,#9322,#9323,#9324,#9325,#9326,
#9327,#9328,#9329,#9330,#9331,#9332,#9333,#9334,#9335,#9336,#9337,#9338,
#9339,#9340,#9341,#9342,#9343,#9344,#9345,#9346,#9347,#9348,#9349,#9350,
#9351,#9352,#9353,#9354,#9355,#9356,#9357,#9358,#9359,#9360,#9361,#9362,
#9363,#9364,#9365,#9366,#9367,#9368,#9369,#9370,#9371,#9372,#9373,#9374,
#9375,#9376,#9377,#9378,#9379,#9380,#9381,#9382,#9383,#9384,#9385,#9386,
#9387),(#9388,#9389,#9390,#9391,#9392,#9393,#9394,#9395,#9396,#9397,#9398,
#9399,#9400,#9401,#9402,#9403,#9404,#9405,#9406,#9407,#9408,#9409,#9410,
#9411,#9412,#9413,#9414,#9415,#9416,#9417,#9418,#9419,#9420,#9421,#9422,
#9423,#9424,#9425,#9426,#9427,#9428,#9429,#9430,#9431,#9432,#9433,#9434,
#9435,#9436,#9437,#9438,#9439,#9440,#9441,#9442,#9443,#9444,#9445,#9446,
#9447,#9448,#9449,#9450,#9451,#9452,#9453,#9454,#9455,#9456,#9457,#9458),
(#9459,#9460,#9461,#9462,#9463,#9464,#9465,#9466,#9467,#9468,#9469,#9470,
#9471,#9472,#9473,#9474,#9475,#9476,#9477,#9478,#9479,#9480,#9481,#9482,
#9483,#9484,#9485,#9486,#9487,#9488,#9489,#9490,#9491,#9492,#9493,#9494,
#9495,#9496,#9497,#9498,#9499,#9500,#9501,#9502,#9503,#9504,#9505,#9506,
#9507,#9508,#9509,#9510,#9511,#9512,#9513,#9514,#9515,#9516,#9517,#9518,
#9519,#9520,#9521,#9522,#9523,#9524,#9525,#9526,#9527,#9528,#9529),(#9530,
#9531,#9532,#9533,#9534,#9535,#9536,#9537,#9538,#9539,#9540,#9541,#9542,
#9543,#9544,#9545,#9546,#9547,#9548,#9549,#9550,#9551,#9552,#9553,#9554,
#9555,#9556,#9557,#9558,#9559,#9560,#9561,#9562,#9563,#9564,#9565,#9566,
#9567,#9568,#9569,#9570,#9571,#9572,#9573,#9574,#9575,#9576,#9577,#9578,
#9579,#9580,#9581,#9582,#9583,#9584,#9585,#9586,#9587,#9588,#9589,#9590,
#9591,#9592,#9593,#9594,#9595,#9596,#9597,#9598,#9599,#9600),(#9601,#9602,
#9603,#9604,#9605,#9606,#9607,#9608,#9609,#9610,#9611,#9612,#9613,#9614,
#9615,#9616,#9617,#9618,#9619,#9620,#9621,#9622,#9623,#9624,#9625,#9626,
#9627,#9628,#9629,#9630,#9631,#9632,#9633,#9634,#9635,#9636,#9637,#9638,
#9639,#9640,#9641,#9642,#9643,#9644,#9645,#9646,#9647,#9648,#9649,#9650,
#9651,#9652,#9653,#9654,#9655,#9656,#9657,#9658,#9659,#9660,#9661,#9662,
#9663,#9664,#9665,#9666,#9667,#9668,#9669,#9670,#9671)),.UNSPECIFIED.,.T.,
 .F.,.F.,(4,1,1,1,1,1,1,4),(4,1,1,1,1,1,1,1,1,1,1,1,1,1,1,1,1,1,1,1,1,1,
1,1,1,1,1,1,1,1,1,1,1,1,1,1,1,1,1,1,1,1,1,1,1,1,1,1,1,1,1,1,1,1,1,1,1,1,
1,1,1,1,1,1,1,1,1,1,4),(-3.14159265358979,-2.24399475256414,-1.34639685153848,
-0.448798950512828,0.448798950512828,1.34639685153848,2.24399475256414,
3.14159265358979),(0.,0.0178571428571429,0.0357142857142857,0.0535714285714286,
0.0714285714285714,0.0892857142857143,0.107142857142857,0.125,0.142857142857143,
0.150793650793651,0.158730158730159,0.174603174603175,0.19047619047619,
0.202380952380952,0.214285714285714,0.226190476190476,0.238095238095238,
0.25,0.261904761904762,0.267857142857143,0.273809523809524,0.285714285714286,
0.297619047619048,0.30952380952381,0.321428571428571,0.333333333333333,
0.349206349206349,0.365079365079365,0.380952380952381,0.396825396825397,
0.412698412698413,0.428571428571429,0.446428571428571,0.464285714285714,
0.476190476190476,0.488095238095238,0.5,0.517857142857143,0.535714285714286,
0.553571428571429,0.571428571428571,0.589285714285714,0.607142857142857,
0.625,0.642857142857143,0.660714285714286,0.678571428571428,0.696428571428571,
0.714285714285714,0.726190476190476,0.738095238095238,0.75,0.761904761904762,
0.773809523809524,0.785714285714286,0.797619047619047,0.809523809523809,
0.821428571428571,0.833333333333333,0.845238095238095,0.857142857142857,
0.875,0.892857142857143,0.910714285714286,0.928571428571429,0.946428571428571,
0.964285714285714,0.982142857142857,1.),.UNSPECIFIED.);
#168=CONICAL_SURFACE('',#5214,0.645,0.785398163397448);
#169=CONICAL_SURFACE('',#5217,0.645,0.785398163397448);
#170=CONICAL_SURFACE('',#5416,0.4,0.785398163397448);
#171=CONICAL_SURFACE('',#5420,0.41,0.785398163397448);
#172=CONICAL_SURFACE('',#5424,0.26,0.463647609000806);
#173=CONICAL_SURFACE('',#5428,0.225,0.785398163397448);
#174=CONICAL_SURFACE('',#5449,0.734027674973257,1.0471975511966);
#175=CONICAL_SURFACE('',#5451,0.734027674973257,1.0471975511966);
#176=CONICAL_SURFACE('',#5474,0.185,0.785398163397449);
#177=CONICAL_SURFACE('',#5478,0.1625,0.785398163397449);
#178=CONICAL_SURFACE('',#5498,0.325,0.785398163397448);
#179=CONICAL_SURFACE('',#5502,0.335,0.785398163397448);
#180=CONICAL_SURFACE('',#5506,0.21,0.463647609000806);
#181=CONICAL_SURFACE('',#5510,0.18,0.785398163397448);
#182=TOROIDAL_SURFACE('',#5115,2.35,0.1);
#183=TOROIDAL_SURFACE('',#5482,0.7495,0.131);
#184=SHAPE_REPRESENTATION_RELATIONSHIP('SRR','None',#10355,#207);
#185=SHAPE_REPRESENTATION_RELATIONSHIP('SRR','None',#10356,#208);
#186=SHAPE_REPRESENTATION_RELATIONSHIP('SRR','None',#10357,#209);
#187=SHAPE_REPRESENTATION_RELATIONSHIP('SRR','None',#10358,#210);
#188=SHAPE_REPRESENTATION_RELATIONSHIP('SRR','None',#10359,#211);
#189=SHAPE_REPRESENTATION_RELATIONSHIP('SRR','None',#10360,#212);
#190=SHAPE_REPRESENTATION_RELATIONSHIP('SRR','None',#10361,#213);
#191=SHAPE_REPRESENTATION_RELATIONSHIP('SRR','None',#10362,#214);
#192=SHAPE_REPRESENTATION_RELATIONSHIP('SRR','None',#10363,#215);
#193=SHAPE_REPRESENTATION_RELATIONSHIP('SRR','None',#10364,#216);
#194=SHAPE_REPRESENTATION_RELATIONSHIP('SRR','None',#10365,#217);
#195=SHAPE_REPRESENTATION_RELATIONSHIP('SRR','None',#10366,#218);
#196=SHAPE_REPRESENTATION_RELATIONSHIP('SRR','None',#10367,#219);
#197=SHAPE_REPRESENTATION_RELATIONSHIP('SRR','None',#10368,#220);
#198=SHAPE_REPRESENTATION_RELATIONSHIP('SRR','None',#10369,#221);
#199=SHAPE_REPRESENTATION_RELATIONSHIP('SRR','None',#10370,#222);
#200=SHAPE_REPRESENTATION_RELATIONSHIP('SRR','None',#10371,#223);
#201=SHAPE_REPRESENTATION_RELATIONSHIP('SRR','None',#10372,#224);
#202=SHAPE_REPRESENTATION_RELATIONSHIP('SRR','None',#10373,#225);
#203=SHAPE_REPRESENTATION_RELATIONSHIP('SRR','None',#10374,#226);
#204=SHAPE_REPRESENTATION_RELATIONSHIP('SRR','None',#10375,#227);
#205=SHAPE_REPRESENTATION_RELATIONSHIP('SRR','None',#10376,#228);
#206=SHAPE_REPRESENTATION_RELATIONSHIP('SRR','None',#10377,#229);
#207=ADVANCED_BREP_SHAPE_REPRESENTATION('',(#255),#10243);
#208=ADVANCED_BREP_SHAPE_REPRESENTATION('',(#256),#10244);
#209=ADVANCED_BREP_SHAPE_REPRESENTATION('',(#257),#10245);
#210=ADVANCED_BREP_SHAPE_REPRESENTATION('',(#258,#259,#260),#10246);
#211=ADVANCED_BREP_SHAPE_REPRESENTATION('',(#261),#10247);
#212=ADVANCED_BREP_SHAPE_REPRESENTATION('',(#262),#10248);
#213=ADVANCED_BREP_SHAPE_REPRESENTATION('',(#263),#10249);
#214=ADVANCED_BREP_SHAPE_REPRESENTATION('',(#264),#10250);
#215=ADVANCED_BREP_SHAPE_REPRESENTATION('',(#265),#10251);
#216=ADVANCED_BREP_SHAPE_REPRESENTATION('',(#266),#10252);
#217=ADVANCED_BREP_SHAPE_REPRESENTATION('',(#267),#10253);
#218=ADVANCED_BREP_SHAPE_REPRESENTATION('',(#268),#10254);
#219=ADVANCED_BREP_SHAPE_REPRESENTATION('',(#269),#10255);
#220=ADVANCED_BREP_SHAPE_REPRESENTATION('',(#270),#10256);
#221=ADVANCED_BREP_SHAPE_REPRESENTATION('',(#271),#10257);
#222=ADVANCED_BREP_SHAPE_REPRESENTATION('',(#272),#10258);
#223=ADVANCED_BREP_SHAPE_REPRESENTATION('',(#165),#10259);
#224=ADVANCED_BREP_SHAPE_REPRESENTATION('',(#273),#10260);
#225=ADVANCED_BREP_SHAPE_REPRESENTATION('',(#274),#10261);
#226=ADVANCED_BREP_SHAPE_REPRESENTATION('',(#275),#10262);
#227=ADVANCED_BREP_SHAPE_REPRESENTATION('',(#276),#10263);
#228=ADVANCED_BREP_SHAPE_REPRESENTATION('',(#277),#10264);
#229=ADVANCED_BREP_SHAPE_REPRESENTATION('',(#166),#10265);
#230=STYLED_ITEM('',(#10526),#255);
#231=STYLED_ITEM('',(#10554),#256);
#232=STYLED_ITEM('',(#10561),#257);
#233=STYLED_ITEM('',(#10561),#258);
#234=STYLED_ITEM('',(#10561),#259);
#235=STYLED_ITEM('',(#10561),#260);
#236=STYLED_ITEM('',(#10526),#261);
#237=STYLED_ITEM('',(#10540),#262);
#238=STYLED_ITEM('',(#10561),#263);
#239=STYLED_ITEM('',(#10561),#264);
#240=STYLED_ITEM('',(#10561),#265);
#241=STYLED_ITEM('',(#10561),#266);
#242=STYLED_ITEM('',(#10540),#267);
#243=STYLED_ITEM('',(#10540),#268);
#244=STYLED_ITEM('',(#10547),#269);
#245=STYLED_ITEM('',(#10547),#270);
#246=STYLED_ITEM('',(#10554),#271);
#247=STYLED_ITEM('',(#10533),#272);
#248=STYLED_ITEM('',(#10554),#165);
#249=STYLED_ITEM('',(#10554),#273);
#250=STYLED_ITEM('',(#10554),#274);
#251=STYLED_ITEM('',(#10554),#275);
#252=STYLED_ITEM('',(#10554),#276);
#253=STYLED_ITEM('',(#10540),#277);
#254=STYLED_ITEM('',(#10554),#166);
#255=MANIFOLD_SOLID_BREP('Body1',#4689);
#256=MANIFOLD_SOLID_BREP('Body1',#4690);
#257=MANIFOLD_SOLID_BREP('Body1',#4691);
#258=MANIFOLD_SOLID_BREP('Body1',#4692);
#259=MANIFOLD_SOLID_BREP('Off white dial',#4693);
#260=MANIFOLD_SOLID_BREP('Black pointer',#4694);
#261=MANIFOLD_SOLID_BREP('Body1',#4695);
#262=MANIFOLD_SOLID_BREP('Body1',#4696);
#263=MANIFOLD_SOLID_BREP('Body1',#4697);
#264=MANIFOLD_SOLID_BREP('Body1',#4698);
#265=MANIFOLD_SOLID_BREP('Body1',#4699);
#266=MANIFOLD_SOLID_BREP('Body1',#4700);
#267=MANIFOLD_SOLID_BREP('Body1',#4701);
#268=MANIFOLD_SOLID_BREP('Body1',#4702);
#269=MANIFOLD_SOLID_BREP('Body1',#4703);
#270=MANIFOLD_SOLID_BREP('Body1',#4704);
#271=MANIFOLD_SOLID_BREP('Body1',#4705);
#272=MANIFOLD_SOLID_BREP('Body1',#4706);
#273=MANIFOLD_SOLID_BREP('Body1',#4709);
#274=MANIFOLD_SOLID_BREP('Body1',#4710);
#275=MANIFOLD_SOLID_BREP('Body1',#4711);
#276=MANIFOLD_SOLID_BREP('Body1',#4712);
#277=MANIFOLD_SOLID_BREP('Body1',#4713);
#278=ELLIPSE('',#5037,0.282842712474619,0.2);
#279=ELLIPSE('',#5038,0.282842712474619,0.2);
#280=ELLIPSE('',#5040,0.282842712474619,0.2);
#281=ELLIPSE('',#5041,0.282842712474619,0.2);
#282=ELLIPSE('',#5043,0.282842712474619,0.2);
#283=ELLIPSE('',#5045,0.282842712474619,0.2);
#284=ELLIPSE('',#5060,0.565685424949238,0.4);
#285=ELLIPSE('',#5061,0.565685424949238,0.4);
#286=ELLIPSE('',#5063,0.565685424949238,0.4);
#287=ELLIPSE('',#5064,0.565685424949238,0.4);
#288=ELLIPSE('',#5067,0.565685424949238,0.4);
#289=ELLIPSE('',#5068,0.565685424949238,0.4);
#290=ELLIPSE('',#5069,0.565685424949238,0.4);
#291=ELLIPSE('',#5070,0.565685424949238,0.4);
#292=FACE_BOUND('',#868,.T.);
#293=FACE_BOUND('',#870,.T.);
#294=FACE_BOUND('',#871,.T.);
#295=FACE_BOUND('',#872,.T.);
#296=FACE_BOUND('',#873,.T.);
#297=FACE_BOUND('',#874,.T.);
#298=FACE_BOUND('',#888,.T.);
#299=FACE_BOUND('',#899,.T.);
#300=FACE_BOUND('',#909,.T.);
#301=FACE_BOUND('',#911,.T.);
#302=FACE_BOUND('',#914,.T.);
#303=FACE_BOUND('',#916,.T.);
#304=FACE_BOUND('',#921,.T.);
#305=FACE_BOUND('',#923,.T.);
#306=FACE_BOUND('',#925,.T.);
#307=FACE_BOUND('',#928,.T.);
#308=FACE_BOUND('',#930,.T.);
#309=FACE_BOUND('',#932,.T.);
#310=FACE_BOUND('',#933,.T.);
#311=FACE_BOUND('',#936,.T.);
#312=FACE_BOUND('',#937,.T.);
#313=FACE_BOUND('',#939,.T.);
#314=FACE_BOUND('',#940,.T.);
#315=FACE_BOUND('',#942,.T.);
#316=FACE_BOUND('',#943,.T.);
#317=FACE_BOUND('',#944,.T.);
#318=FACE_BOUND('',#945,.T.);
#319=FACE_BOUND('',#946,.T.);
#320=FACE_BOUND('',#947,.T.);
#321=FACE_BOUND('',#948,.T.);
#322=FACE_BOUND('',#950,.T.);
#323=FACE_BOUND('',#951,.T.);
#324=FACE_BOUND('',#952,.T.);
#325=FACE_BOUND('',#967,.T.);
#326=FACE_BOUND('',#968,.T.);
#327=FACE_BOUND('',#969,.T.);
#328=FACE_BOUND('',#970,.T.);
#329=FACE_BOUND('',#971,.T.);
#330=FACE_BOUND('',#972,.T.);
#331=FACE_BOUND('',#973,.T.);
#332=FACE_BOUND('',#974,.T.);
#333=FACE_BOUND('',#975,.T.);
#334=FACE_BOUND('',#979,.T.);
#335=FACE_BOUND('',#981,.T.);
#336=FACE_BOUND('',#982,.T.);
#337=FACE_BOUND('',#983,.T.);
#338=FACE_BOUND('',#984,.T.);
#339=FACE_BOUND('',#985,.T.);
#340=FACE_BOUND('',#986,.T.);
#341=FACE_BOUND('',#987,.T.);
#342=FACE_BOUND('',#988,.T.);
#343=FACE_BOUND('',#989,.T.);
#344=FACE_BOUND('',#991,.T.);
#345=FACE_BOUND('',#994,.T.);
#346=FACE_BOUND('',#1016,.T.);
#347=FACE_BOUND('',#1017,.T.);
#348=FACE_BOUND('',#1019,.T.);
#349=FACE_BOUND('',#1020,.T.);
#350=FACE_BOUND('',#1024,.T.);
#351=FACE_BOUND('',#1025,.T.);
#352=FACE_BOUND('',#1026,.T.);
#353=FACE_BOUND('',#1027,.T.);
#354=FACE_BOUND('',#1033,.T.);
#355=FACE_BOUND('',#1034,.T.);
#356=FACE_BOUND('',#1035,.T.);
#357=FACE_BOUND('',#1037,.T.);
#358=FACE_BOUND('',#1038,.T.);
#359=FACE_BOUND('',#1039,.T.);
#360=FACE_BOUND('',#1041,.T.);
#361=FACE_BOUND('',#1043,.T.);
#362=FACE_BOUND('',#1052,.T.);
#363=FACE_BOUND('',#1057,.T.);
#364=FACE_BOUND('',#1062,.T.);
#365=FACE_BOUND('',#1064,.T.);
#366=FACE_BOUND('',#1066,.T.);
#367=FACE_BOUND('',#1069,.T.);
#368=FACE_BOUND('',#1071,.T.);
#369=FACE_BOUND('',#1078,.T.);
#370=FACE_BOUND('',#1083,.T.);
#371=FACE_BOUND('',#1085,.T.);
#372=FACE_BOUND('',#1095,.T.);
#373=FACE_BOUND('',#1096,.T.);
#374=FACE_BOUND('',#1097,.T.);
#375=FACE_BOUND('',#1098,.T.);
#376=FACE_BOUND('',#1099,.T.);
#377=FACE_BOUND('',#1100,.T.);
#378=FACE_BOUND('',#1101,.T.);
#379=FACE_BOUND('',#1103,.T.);
#380=FACE_BOUND('',#1104,.T.);
#381=FACE_BOUND('',#1105,.T.);
#382=FACE_BOUND('',#1106,.T.);
#383=FACE_BOUND('',#1107,.T.);
#384=FACE_BOUND('',#1108,.T.);
#385=FACE_BOUND('',#1109,.T.);
#386=FACE_BOUND('',#1113,.T.);
#387=FACE_BOUND('',#1115,.T.);
#388=FACE_BOUND('',#1119,.T.);
#389=FACE_BOUND('',#1121,.T.);
#390=FACE_BOUND('',#1144,.T.);
#391=FACE_BOUND('',#1146,.T.);
#392=FACE_BOUND('',#1149,.T.);
#393=FACE_BOUND('',#1150,.T.);
#394=FACE_BOUND('',#1151,.T.);
#395=FACE_BOUND('',#1152,.T.);
#396=FACE_BOUND('',#1153,.T.);
#397=FACE_BOUND('',#1154,.T.);
#398=FACE_BOUND('',#1155,.T.);
#399=FACE_BOUND('',#1157,.T.);
#400=FACE_BOUND('',#1158,.T.);
#401=FACE_BOUND('',#1159,.T.);
#402=FACE_BOUND('',#1160,.T.);
#403=FACE_BOUND('',#1161,.T.);
#404=FACE_BOUND('',#1162,.T.);
#405=FACE_BOUND('',#1163,.T.);
#406=FACE_BOUND('',#1172,.T.);
#407=FACE_BOUND('',#1180,.T.);
#408=FACE_BOUND('',#1182,.T.);
#409=FACE_BOUND('',#1184,.T.);
#410=FACE_BOUND('',#1186,.T.);
#411=FACE_BOUND('',#1192,.T.);
#412=FACE_BOUND('',#1208,.T.);
#413=FACE_BOUND('',#1210,.T.);
#414=FACE_BOUND('',#1221,.T.);
#415=FACE_BOUND('',#1223,.T.);
#416=FACE_BOUND('',#1232,.T.);
#417=FACE_BOUND('',#1244,.T.);
#418=FACE_BOUND('',#1246,.T.);
#419=FACE_BOUND('',#1252,.T.);
#420=PLANE('',#4977);
#421=PLANE('',#4981);
#422=PLANE('',#4985);
#423=PLANE('',#4989);
#424=PLANE('',#4993);
#425=PLANE('',#5000);
#426=PLANE('',#5001);
#427=PLANE('',#5003);
#428=PLANE('',#5011);
#429=PLANE('',#5015);
#430=PLANE('',#5019);
#431=PLANE('',#5023);
#432=PLANE('',#5027);
#433=PLANE('',#5028);
#434=PLANE('',#5032);
#435=PLANE('',#5034);
#436=PLANE('',#5052);
#437=PLANE('',#5053);
#438=PLANE('',#5055);
#439=PLANE('',#5057);
#440=PLANE('',#5071);
#441=PLANE('',#5078);
#442=PLANE('',#5082);
#443=PLANE('',#5084);
#444=PLANE('',#5093);
#445=PLANE('',#5095);
#446=PLANE('',#5101);
#447=PLANE('',#5105);
#448=PLANE('',#5108);
#449=PLANE('',#5112);
#450=PLANE('',#5113);
#451=PLANE('',#5134);
#452=PLANE('',#5138);
#453=PLANE('',#5142);
#454=PLANE('',#5143);
#455=PLANE('',#5145);
#456=PLANE('',#5150);
#457=PLANE('',#5153);
#458=PLANE('',#5157);
#459=PLANE('',#5158);
#460=PLANE('',#5159);
#461=PLANE('',#5160);
#462=PLANE('',#5161);
#463=PLANE('',#5162);
#464=PLANE('',#5163);
#465=PLANE('',#5164);
#466=PLANE('',#5165);
#467=PLANE('',#5185);
#468=PLANE('',#5186);
#469=PLANE('',#5187);
#470=PLANE('',#5188);
#471=PLANE('',#5189);
#472=PLANE('',#5193);
#473=PLANE('',#5194);
#474=PLANE('',#5195);
#475=PLANE('',#5196);
#476=PLANE('',#5197);
#477=PLANE('',#5199);
#478=PLANE('',#5201);
#479=PLANE('',#5203);
#480=PLANE('',#5204);
#481=PLANE('',#5205);
#482=PLANE('',#5206);
#483=PLANE('',#5207);
#484=PLANE('',#5208);
#485=PLANE('',#5211);
#486=PLANE('',#5219);
#487=PLANE('',#5229);
#488=PLANE('',#5230);
#489=PLANE('',#5232);
#490=PLANE('',#5237);
#491=PLANE('',#5240);
#492=PLANE('',#5247);
#493=PLANE('',#5251);
#494=PLANE('',#5252);
#495=PLANE('',#5260);
#496=PLANE('',#5261);
#497=PLANE('',#5287);
#498=PLANE('',#5288);
#499=PLANE('',#5296);
#500=PLANE('',#5297);
#501=PLANE('',#5304);
#502=PLANE('',#5305);
#503=PLANE('',#5307);
#504=PLANE('',#5315);
#505=PLANE('',#5317);
#506=PLANE('',#5322);
#507=PLANE('',#5327);
#508=PLANE('',#5335);
#509=PLANE('',#5370);
#510=PLANE('',#5371);
#511=PLANE('',#5375);
#512=PLANE('',#5376);
#513=PLANE('',#5380);
#514=PLANE('',#5381);
#515=PLANE('',#5386);
#516=PLANE('',#5390);
#517=PLANE('',#5391);
#518=PLANE('',#5396);
#519=PLANE('',#5397);
#520=PLANE('',#5399);
#521=PLANE('',#5404);
#522=PLANE('',#5411);
#523=PLANE('',#5412);
#524=PLANE('',#5414);
#525=PLANE('',#5422);
#526=PLANE('',#5430);
#527=PLANE('',#5431);
#528=PLANE('',#5432);
#529=PLANE('',#5433);
#530=PLANE('',#5434);
#531=PLANE('',#5435);
#532=PLANE('',#5436);
#533=PLANE('',#5437);
#534=PLANE('',#5438);
#535=PLANE('',#5446);
#536=PLANE('',#5447);
#537=PLANE('',#5453);
#538=PLANE('',#5454);
#539=PLANE('',#5455);
#540=PLANE('',#5459);
#541=PLANE('',#5460);
#542=PLANE('',#5461);
#543=PLANE('',#5462);
#544=PLANE('',#5463);
#545=PLANE('',#5465);
#546=PLANE('',#5466);
#547=PLANE('',#5467);
#548=PLANE('',#5468);
#549=PLANE('',#5469);
#550=PLANE('',#5470);
#551=PLANE('',#5471);
#552=PLANE('',#5472);
#553=PLANE('',#5480);
#554=PLANE('',#5489);
#555=PLANE('',#5490);
#556=PLANE('',#5491);
#557=PLANE('',#5492);
#558=PLANE('',#5493);
#559=PLANE('',#5494);
#560=PLANE('',#5496);
#561=PLANE('',#5504);
#562=PLANE('',#5512);
#563=PLANE('',#5513);
#564=PLANE('',#5514);
#565=PLANE('',#5515);
#566=PLANE('',#5516);
#567=PLANE('',#5517);
#568=PLANE('',#5518);
#569=PLANE('',#5519);
#570=PLANE('',#5520);
#571=FACE_OUTER_BOUND('',#854,.T.);
#572=FACE_OUTER_BOUND('',#855,.T.);
#573=FACE_OUTER_BOUND('',#856,.T.);
#574=FACE_OUTER_BOUND('',#857,.T.);
#575=FACE_OUTER_BOUND('',#858,.T.);
#576=FACE_OUTER_BOUND('',#859,.T.);
#577=FACE_OUTER_BOUND('',#860,.T.);
#578=FACE_OUTER_BOUND('',#861,.T.);
#579=FACE_OUTER_BOUND('',#862,.T.);
#580=FACE_OUTER_BOUND('',#863,.T.);
#581=FACE_OUTER_BOUND('',#864,.T.);
#582=FACE_OUTER_BOUND('',#865,.T.);
#583=FACE_OUTER_BOUND('',#866,.T.);
#584=FACE_OUTER_BOUND('',#867,.T.);
#585=FACE_OUTER_BOUND('',#869,.T.);
#586=FACE_OUTER_BOUND('',#875,.T.);
#587=FACE_OUTER_BOUND('',#876,.T.);
#588=FACE_OUTER_BOUND('',#877,.T.);
#589=FACE_OUTER_BOUND('',#878,.T.);
#590=FACE_OUTER_BOUND('',#879,.T.);
#591=FACE_OUTER_BOUND('',#880,.T.);
#592=FACE_OUTER_BOUND('',#881,.T.);
#593=FACE_OUTER_BOUND('',#882,.T.);
#594=FACE_OUTER_BOUND('',#883,.T.);
#595=FACE_OUTER_BOUND('',#884,.T.);
#596=FACE_OUTER_BOUND('',#885,.T.);
#597=FACE_OUTER_BOUND('',#886,.T.);
#598=FACE_OUTER_BOUND('',#887,.T.);
#599=FACE_OUTER_BOUND('',#889,.T.);
#600=FACE_OUTER_BOUND('',#890,.T.);
#601=FACE_OUTER_BOUND('',#891,.T.);
#602=FACE_OUTER_BOUND('',#892,.T.);
#603=FACE_OUTER_BOUND('',#893,.T.);
#604=FACE_OUTER_BOUND('',#894,.T.);
#605=FACE_OUTER_BOUND('',#895,.T.);
#606=FACE_OUTER_BOUND('',#896,.T.);
#607=FACE_OUTER_BOUND('',#897,.T.);
#608=FACE_OUTER_BOUND('',#898,.T.);
#609=FACE_OUTER_BOUND('',#900,.T.);
#610=FACE_OUTER_BOUND('',#901,.T.);
#611=FACE_OUTER_BOUND('',#902,.T.);
#612=FACE_OUTER_BOUND('',#903,.T.);
#613=FACE_OUTER_BOUND('',#904,.T.);
#614=FACE_OUTER_BOUND('',#905,.T.);
#615=FACE_OUTER_BOUND('',#906,.T.);
#616=FACE_OUTER_BOUND('',#907,.T.);
#617=FACE_OUTER_BOUND('',#908,.T.);
#618=FACE_OUTER_BOUND('',#910,.T.);
#619=FACE_OUTER_BOUND('',#912,.T.);
#620=FACE_OUTER_BOUND('',#913,.T.);
#621=FACE_OUTER_BOUND('',#915,.T.);
#622=FACE_OUTER_BOUND('',#917,.T.);
#623=FACE_OUTER_BOUND('',#918,.T.);
#624=FACE_OUTER_BOUND('',#919,.T.);
#625=FACE_OUTER_BOUND('',#920,.T.);
#626=FACE_OUTER_BOUND('',#922,.T.);
#627=FACE_OUTER_BOUND('',#924,.T.);
#628=FACE_OUTER_BOUND('',#926,.T.);
#629=FACE_OUTER_BOUND('',#927,.T.);
#630=FACE_OUTER_BOUND('',#929,.T.);
#631=FACE_OUTER_BOUND('',#931,.T.);
#632=FACE_OUTER_BOUND('',#934,.T.);
#633=FACE_OUTER_BOUND('',#935,.T.);
#634=FACE_OUTER_BOUND('',#938,.T.);
#635=FACE_OUTER_BOUND('',#941,.T.);
#636=FACE_OUTER_BOUND('',#949,.T.);
#637=FACE_OUTER_BOUND('',#953,.T.);
#638=FACE_OUTER_BOUND('',#954,.T.);
#639=FACE_OUTER_BOUND('',#955,.T.);
#640=FACE_OUTER_BOUND('',#956,.T.);
#641=FACE_OUTER_BOUND('',#957,.T.);
#642=FACE_OUTER_BOUND('',#958,.T.);
#643=FACE_OUTER_BOUND('',#959,.T.);
#644=FACE_OUTER_BOUND('',#960,.T.);
#645=FACE_OUTER_BOUND('',#961,.T.);
#646=FACE_OUTER_BOUND('',#962,.T.);
#647=FACE_OUTER_BOUND('',#963,.T.);
#648=FACE_OUTER_BOUND('',#964,.T.);
#649=FACE_OUTER_BOUND('',#965,.T.);
#650=FACE_OUTER_BOUND('',#966,.T.);
#651=FACE_OUTER_BOUND('',#976,.T.);
#652=FACE_OUTER_BOUND('',#977,.T.);
#653=FACE_OUTER_BOUND('',#978,.T.);
#654=FACE_OUTER_BOUND('',#980,.T.);
#655=FACE_OUTER_BOUND('',#990,.T.);
#656=FACE_OUTER_BOUND('',#992,.T.);
#657=FACE_OUTER_BOUND('',#993,.T.);
#658=FACE_OUTER_BOUND('',#995,.T.);
#659=FACE_OUTER_BOUND('',#996,.T.);
#660=FACE_OUTER_BOUND('',#997,.T.);
#661=FACE_OUTER_BOUND('',#998,.T.);
#662=FACE_OUTER_BOUND('',#999,.T.);
#663=FACE_OUTER_BOUND('',#1000,.T.);
#664=FACE_OUTER_BOUND('',#1001,.T.);
#665=FACE_OUTER_BOUND('',#1002,.T.);
#666=FACE_OUTER_BOUND('',#1003,.T.);
#667=FACE_OUTER_BOUND('',#1004,.T.);
#668=FACE_OUTER_BOUND('',#1005,.T.);
#669=FACE_OUTER_BOUND('',#1006,.T.);
#670=FACE_OUTER_BOUND('',#1007,.T.);
#671=FACE_OUTER_BOUND('',#1008,.T.);
#672=FACE_OUTER_BOUND('',#1009,.T.);
#673=FACE_OUTER_BOUND('',#1010,.T.);
#674=FACE_OUTER_BOUND('',#1011,.T.);
#675=FACE_OUTER_BOUND('',#1012,.T.);
#676=FACE_OUTER_BOUND('',#1013,.T.);
#677=FACE_OUTER_BOUND('',#1014,.T.);
#678=FACE_OUTER_BOUND('',#1015,.T.);
#679=FACE_OUTER_BOUND('',#1018,.T.);
#680=FACE_OUTER_BOUND('',#1021,.T.);
#681=FACE_OUTER_BOUND('',#1022,.T.);
#682=FACE_OUTER_BOUND('',#1023,.T.);
#683=FACE_OUTER_BOUND('',#1028,.T.);
#684=FACE_OUTER_BOUND('',#1029,.T.);
#685=FACE_OUTER_BOUND('',#1030,.T.);
#686=FACE_OUTER_BOUND('',#1031,.T.);
#687=FACE_OUTER_BOUND('',#1032,.T.);
#688=FACE_OUTER_BOUND('',#1036,.T.);
#689=FACE_OUTER_BOUND('',#1040,.T.);
#690=FACE_OUTER_BOUND('',#1042,.T.);
#691=FACE_OUTER_BOUND('',#1044,.T.);
#692=FACE_OUTER_BOUND('',#1045,.T.);
#693=FACE_OUTER_BOUND('',#1046,.T.);
#694=FACE_OUTER_BOUND('',#1047,.T.);
#695=FACE_OUTER_BOUND('',#1048,.T.);
#696=FACE_OUTER_BOUND('',#1049,.T.);
#697=FACE_OUTER_BOUND('',#1050,.T.);
#698=FACE_OUTER_BOUND('',#1051,.T.);
#699=FACE_OUTER_BOUND('',#1053,.T.);
#700=FACE_OUTER_BOUND('',#1054,.T.);
#701=FACE_OUTER_BOUND('',#1055,.T.);
#702=FACE_OUTER_BOUND('',#1056,.T.);
#703=FACE_OUTER_BOUND('',#1058,.T.);
#704=FACE_OUTER_BOUND('',#1059,.T.);
#705=FACE_OUTER_BOUND('',#1060,.T.);
#706=FACE_OUTER_BOUND('',#1061,.T.);
#707=FACE_OUTER_BOUND('',#1063,.T.);
#708=FACE_OUTER_BOUND('',#1065,.T.);
#709=FACE_OUTER_BOUND('',#1067,.T.);
#710=FACE_OUTER_BOUND('',#1068,.T.);
#711=FACE_OUTER_BOUND('',#1070,.T.);
#712=FACE_OUTER_BOUND('',#1072,.T.);
#713=FACE_OUTER_BOUND('',#1073,.T.);
#714=FACE_OUTER_BOUND('',#1074,.T.);
#715=FACE_OUTER_BOUND('',#1075,.T.);
#716=FACE_OUTER_BOUND('',#1076,.T.);
#717=FACE_OUTER_BOUND('',#1077,.T.);
#718=FACE_OUTER_BOUND('',#1079,.T.);
#719=FACE_OUTER_BOUND('',#1080,.T.);
#720=FACE_OUTER_BOUND('',#1081,.T.);
#721=FACE_OUTER_BOUND('',#1082,.T.);
#722=FACE_OUTER_BOUND('',#1084,.T.);
#723=FACE_OUTER_BOUND('',#1086,.T.);
#724=FACE_OUTER_BOUND('',#1087,.T.);
#725=FACE_OUTER_BOUND('',#1088,.T.);
#726=FACE_OUTER_BOUND('',#1089,.T.);
#727=FACE_OUTER_BOUND('',#1090,.T.);
#728=FACE_OUTER_BOUND('',#1091,.T.);
#729=FACE_OUTER_BOUND('',#1092,.T.);
#730=FACE_OUTER_BOUND('',#1093,.T.);
#731=FACE_OUTER_BOUND('',#1094,.T.);
#732=FACE_OUTER_BOUND('',#1102,.T.);
#733=FACE_OUTER_BOUND('',#1110,.T.);
#734=FACE_OUTER_BOUND('',#1111,.T.);
#735=FACE_OUTER_BOUND('',#1112,.T.);
#736=FACE_OUTER_BOUND('',#1114,.T.);
#737=FACE_OUTER_BOUND('',#1116,.T.);
#738=FACE_OUTER_BOUND('',#1117,.T.);
#739=FACE_OUTER_BOUND('',#1118,.T.);
#740=FACE_OUTER_BOUND('',#1120,.T.);
#741=FACE_OUTER_BOUND('',#1122,.T.);
#742=FACE_OUTER_BOUND('',#1123,.T.);
#743=FACE_OUTER_BOUND('',#1124,.T.);
#744=FACE_OUTER_BOUND('',#1125,.T.);
#745=FACE_OUTER_BOUND('',#1126,.T.);
#746=FACE_OUTER_BOUND('',#1127,.T.);
#747=FACE_OUTER_BOUND('',#1128,.T.);
#748=FACE_OUTER_BOUND('',#1129,.T.);
#749=FACE_OUTER_BOUND('',#1130,.T.);
#750=FACE_OUTER_BOUND('',#1131,.T.);
#751=FACE_OUTER_BOUND('',#1132,.T.);
#752=FACE_OUTER_BOUND('',#1133,.T.);
#753=FACE_OUTER_BOUND('',#1134,.T.);
#754=FACE_OUTER_BOUND('',#1135,.T.);
#755=FACE_OUTER_BOUND('',#1136,.T.);
#756=FACE_OUTER_BOUND('',#1137,.T.);
#757=FACE_OUTER_BOUND('',#1138,.T.);
#758=FACE_OUTER_BOUND('',#1139,.T.);
#759=FACE_OUTER_BOUND('',#1140,.T.);
#760=FACE_OUTER_BOUND('',#1141,.T.);
#761=FACE_OUTER_BOUND('',#1142,.T.);
#762=FACE_OUTER_BOUND('',#1143,.T.);
#763=FACE_OUTER_BOUND('',#1145,.T.);
#764=FACE_OUTER_BOUND('',#1147,.T.);
#765=FACE_OUTER_BOUND('',#1148,.T.);
#766=FACE_OUTER_BOUND('',#1156,.T.);
#767=FACE_OUTER_BOUND('',#1164,.T.);
#768=FACE_OUTER_BOUND('',#1165,.T.);
#769=FACE_OUTER_BOUND('',#1166,.T.);
#770=FACE_OUTER_BOUND('',#1167,.T.);
#771=FACE_OUTER_BOUND('',#1168,.T.);
#772=FACE_OUTER_BOUND('',#1169,.T.);
#773=FACE_OUTER_BOUND('',#1170,.T.);
#774=FACE_OUTER_BOUND('',#1171,.T.);
#775=FACE_OUTER_BOUND('',#1173,.T.);
#776=FACE_OUTER_BOUND('',#1174,.T.);
#777=FACE_OUTER_BOUND('',#1175,.T.);
#778=FACE_OUTER_BOUND('',#1176,.T.);
#779=FACE_OUTER_BOUND('',#1177,.T.);
#780=FACE_OUTER_BOUND('',#1178,.T.);
#781=FACE_OUTER_BOUND('',#1179,.T.);
#782=FACE_OUTER_BOUND('',#1181,.T.);
#783=FACE_OUTER_BOUND('',#1183,.T.);
#784=FACE_OUTER_BOUND('',#1185,.T.);
#785=FACE_OUTER_BOUND('',#1187,.T.);
#786=FACE_OUTER_BOUND('',#1188,.T.);
#787=FACE_OUTER_BOUND('',#1189,.T.);
#788=FACE_OUTER_BOUND('',#1190,.T.);
#789=FACE_OUTER_BOUND('',#1191,.T.);
#790=FACE_OUTER_BOUND('',#1193,.T.);
#791=FACE_OUTER_BOUND('',#1194,.T.);
#792=FACE_OUTER_BOUND('',#1195,.T.);
#793=FACE_OUTER_BOUND('',#1196,.T.);
#794=FACE_OUTER_BOUND('',#1197,.T.);
#795=FACE_OUTER_BOUND('',#1198,.T.);
#796=FACE_OUTER_BOUND('',#1199,.T.);
#797=FACE_OUTER_BOUND('',#1200,.T.);
#798=FACE_OUTER_BOUND('',#1201,.T.);
#799=FACE_OUTER_BOUND('',#1202,.T.);
#800=FACE_OUTER_BOUND('',#1203,.T.);
#801=FACE_OUTER_BOUND('',#1204,.T.);
#802=FACE_OUTER_BOUND('',#1205,.T.);
#803=FACE_OUTER_BOUND('',#1206,.T.);
#804=FACE_OUTER_BOUND('',#1207,.T.);
#805=FACE_OUTER_BOUND('',#1209,.T.);
#806=FACE_OUTER_BOUND('',#1211,.T.);
#807=FACE_OUTER_BOUND('',#1212,.T.);
#808=FACE_OUTER_BOUND('',#1213,.T.);
#809=FACE_OUTER_BOUND('',#1214,.T.);
#810=FACE_OUTER_BOUND('',#1215,.T.);
#811=FACE_OUTER_BOUND('',#1216,.T.);
#812=FACE_OUTER_BOUND('',#1217,.T.);
#813=FACE_OUTER_BOUND('',#1218,.T.);
#814=FACE_OUTER_BOUND('',#1219,.T.);
#815=FACE_OUTER_BOUND('',#1220,.T.);
#816=FACE_OUTER_BOUND('',#1222,.T.);
#817=FACE_OUTER_BOUND('',#1224,.T.);
#818=FACE_OUTER_BOUND('',#1225,.T.);
#819=FACE_OUTER_BOUND('',#1226,.T.);
#820=FACE_OUTER_BOUND('',#1227,.T.);
#821=FACE_OUTER_BOUND('',#1228,.T.);
#822=FACE_OUTER_BOUND('',#1229,.T.);
#823=FACE_OUTER_BOUND('',#1230,.T.);
#824=FACE_OUTER_BOUND('',#1231,.T.);
#825=FACE_OUTER_BOUND('',#1233,.T.);
#826=FACE_OUTER_BOUND('',#1234,.T.);
#827=FACE_OUTER_BOUND('',#1235,.T.);
#828=FACE_OUTER_BOUND('',#1236,.T.);
#829=FACE_OUTER_BOUND('',#1237,.T.);
#830=FACE_OUTER_BOUND('',#1238,.T.);
#831=FACE_OUTER_BOUND('',#1239,.T.);
#832=FACE_OUTER_BOUND('',#1240,.T.);
#833=FACE_OUTER_BOUND('',#1241,.T.);
#834=FACE_OUTER_BOUND('',#1242,.T.);
#835=FACE_OUTER_BOUND('',#1243,.T.);
#836=FACE_OUTER_BOUND('',#1245,.T.);
#837=FACE_OUTER_BOUND('',#1247,.T.);
#838=FACE_OUTER_BOUND('',#1248,.T.);
#839=FACE_OUTER_BOUND('',#1249,.T.);
#840=FACE_OUTER_BOUND('',#1250,.T.);
#841=FACE_OUTER_BOUND('',#1251,.T.);
#842=FACE_OUTER_BOUND('',#1253,.T.);
#843=FACE_OUTER_BOUND('',#1254,.T.);
#844=FACE_OUTER_BOUND('',#1255,.T.);
#845=FACE_OUTER_BOUND('',#1256,.T.);
#846=FACE_OUTER_BOUND('',#1257,.T.);
#847=FACE_OUTER_BOUND('',#1258,.T.);
#848=FACE_OUTER_BOUND('',#1259,.T.);
#849=FACE_OUTER_BOUND('',#1260,.T.);
#850=FACE_OUTER_BOUND('',#1261,.T.);
#851=FACE_OUTER_BOUND('',#1262,.T.);
#852=FACE_OUTER_BOUND('',#1263,.T.);
#853=FACE_OUTER_BOUND('',#1264,.T.);
#854=EDGE_LOOP('',(#3101,#3102,#3103,#3104,#3105));
#855=EDGE_LOOP('',(#3106,#3107,#3108,#3109));
#856=EDGE_LOOP('',(#3110));
#857=EDGE_LOOP('',(#3111,#3112,#3113,#3114));
#858=EDGE_LOOP('',(#3115));
#859=EDGE_LOOP('',(#3116,#3117,#3118,#3119));
#860=EDGE_LOOP('',(#3120));
#861=EDGE_LOOP('',(#3121,#3122,#3123,#3124));
#862=EDGE_LOOP('',(#3125));
#863=EDGE_LOOP('',(#3126,#3127,#3128,#3129));
#864=EDGE_LOOP('',(#3130));
#865=EDGE_LOOP('',(#3131,#3132,#3133,#3134));
#866=EDGE_LOOP('',(#3135,#3136,#3137,#3138));
#867=EDGE_LOOP('',(#3139));
#868=EDGE_LOOP('',(#3140));
#869=EDGE_LOOP('',(#3141));
#870=EDGE_LOOP('',(#3142));
#871=EDGE_LOOP('',(#3143));
#872=EDGE_LOOP('',(#3144));
#873=EDGE_LOOP('',(#3145));
#874=EDGE_LOOP('',(#3146));
#875=EDGE_LOOP('',(#3147,#3148,#3149));
#876=EDGE_LOOP('',(#3150,#3151,#3152,#3153,#3154,#3155,#3156,#3157));
#877=EDGE_LOOP('',(#3158,#3159,#3160,#3161));
#878=EDGE_LOOP('',(#3162));
#879=EDGE_LOOP('',(#3163,#3164,#3165,#3166));
#880=EDGE_LOOP('',(#3167));
#881=EDGE_LOOP('',(#3168,#3169,#3170,#3171));
#882=EDGE_LOOP('',(#3172));
#883=EDGE_LOOP('',(#3173,#3174,#3175,#3176));
#884=EDGE_LOOP('',(#3177));
#885=EDGE_LOOP('',(#3178,#3179,#3180,#3181));
#886=EDGE_LOOP('',(#3182));
#887=EDGE_LOOP('',(#3183,#3184,#3185,#3186,#3187));
#888=EDGE_LOOP('',(#3188));
#889=EDGE_LOOP('',(#3189,#3190));
#890=EDGE_LOOP('',(#3191,#3192));
#891=EDGE_LOOP('',(#3193,#3194,#3195));
#892=EDGE_LOOP('',(#3196,#3197,#3198));
#893=EDGE_LOOP('',(#3199,#3200,#3201,#3202,#3203));
#894=EDGE_LOOP('',(#3204,#3205,#3206,#3207,#3208,#3209,#3210,#3211,#3212,
#3213,#3214,#3215,#3216,#3217));
#895=EDGE_LOOP('',(#3218,#3219,#3220,#3221,#3222,#3223));
#896=EDGE_LOOP('',(#3224,#3225,#3226,#3227,#3228));
#897=EDGE_LOOP('',(#3229,#3230,#3231,#3232,#3233));
#898=EDGE_LOOP('',(#3234));
#899=EDGE_LOOP('',(#3235));
#900=EDGE_LOOP('',(#3236,#3237));
#901=EDGE_LOOP('',(#3238,#3239));
#902=EDGE_LOOP('',(#3240,#3241));
#903=EDGE_LOOP('',(#3242,#3243,#3244));
#904=EDGE_LOOP('',(#3245,#3246,#3247));
#905=EDGE_LOOP('',(#3248,#3249,#3250,#3251,#3252,#3253,#3254,#3255,#3256,
#3257));
#906=EDGE_LOOP('',(#3258,#3259,#3260,#3261,#3262));
#907=EDGE_LOOP('',(#3263,#3264,#3265,#3266,#3267,#3268,#3269,#3270,#3271,
#3272,#3273,#3274,#3275,#3276,#3277));
#908=EDGE_LOOP('',(#3278,#3279,#3280,#3281,#3282,#3283));
#909=EDGE_LOOP('',(#3284,#3285));
#910=EDGE_LOOP('',(#3286));
#911=EDGE_LOOP('',(#3287));
#912=EDGE_LOOP('',(#3288,#3289,#3290,#3291));
#913=EDGE_LOOP('',(#3292));
#914=EDGE_LOOP('',(#3293));
#915=EDGE_LOOP('',(#3294));
#916=EDGE_LOOP('',(#3295));
#917=EDGE_LOOP('',(#3296,#3297,#3298,#3299));
#918=EDGE_LOOP('',(#3300,#3301,#3302,#3303));
#919=EDGE_LOOP('',(#3304,#3305,#3306,#3307));
#920=EDGE_LOOP('',(#3308));
#921=EDGE_LOOP('',(#3309));
#922=EDGE_LOOP('',(#3310));
#923=EDGE_LOOP('',(#3311));
#924=EDGE_LOOP('',(#3312,#3313,#3314,#3315));
#925=EDGE_LOOP('',(#3316));
#926=EDGE_LOOP('',(#3317,#3318,#3319,#3320));
#927=EDGE_LOOP('',(#3321));
#928=EDGE_LOOP('',(#3322));
#929=EDGE_LOOP('',(#3323,#3324,#3325,#3326));
#930=EDGE_LOOP('',(#3327,#3328));
#931=EDGE_LOOP('',(#3329));
#932=EDGE_LOOP('',(#3330));
#933=EDGE_LOOP('',(#3331));
#934=EDGE_LOOP('',(#3332,#3333,#3334,#3335));
#935=EDGE_LOOP('',(#3336));
#936=EDGE_LOOP('',(#3337));
#937=EDGE_LOOP('',(#3338));
#938=EDGE_LOOP('',(#3339,#3340,#3341,#3342,#3343,#3344,#3345,#3346,#3347));
#939=EDGE_LOOP('',(#3348));
#940=EDGE_LOOP('',(#3349,#3350));
#941=EDGE_LOOP('',(#3351));
#942=EDGE_LOOP('',(#3352));
#943=EDGE_LOOP('',(#3353));
#944=EDGE_LOOP('',(#3354));
#945=EDGE_LOOP('',(#3355));
#946=EDGE_LOOP('',(#3356));
#947=EDGE_LOOP('',(#3357));
#948=EDGE_LOOP('',(#3358));
#949=EDGE_LOOP('',(#3359));
#950=EDGE_LOOP('',(#3360));
#951=EDGE_LOOP('',(#3361));
#952=EDGE_LOOP('',(#3362));
#953=EDGE_LOOP('',(#3363,#3364,#3365,#3366));
#954=EDGE_LOOP('',(#3367,#3368,#3369,#3370));
#955=EDGE_LOOP('',(#3371,#3372,#3373,#3374));
#956=EDGE_LOOP('',(#3375,#3376,#3377,#3378));
#957=EDGE_LOOP('',(#3379,#3380,#3381,#3382));
#958=EDGE_LOOP('',(#3383,#3384,#3385,#3386));
#959=EDGE_LOOP('',(#3387,#3388,#3389,#3390));
#960=EDGE_LOOP('',(#3391,#3392,#3393,#3394,#3395,#3396,#3397,#3398));
#961=EDGE_LOOP('',(#3399,#3400,#3401,#3402,#3403,#3404));
#962=EDGE_LOOP('',(#3405,#3406,#3407,#3408,#3409,#3410,#3411,#3412));
#963=EDGE_LOOP('',(#3413,#3414,#3415,#3416,#3417,#3418));
#964=EDGE_LOOP('',(#3419,#3420,#3421,#3422,#3423,#3424,#3425,#3426));
#965=EDGE_LOOP('',(#3427,#3428,#3429,#3430,#3431,#3432));
#966=EDGE_LOOP('',(#3433,#3434,#3435,#3436,#3437,#3438,#3439,#3440,#3441,
#3442,#3443,#3444,#3445,#3446,#3447,#3448,#3449,#3450,#3451));
#967=EDGE_LOOP('',(#3452));
#968=EDGE_LOOP('',(#3453));
#969=EDGE_LOOP('',(#3454));
#970=EDGE_LOOP('',(#3455));
#971=EDGE_LOOP('',(#3456));
#972=EDGE_LOOP('',(#3457));
#973=EDGE_LOOP('',(#3458,#3459));
#974=EDGE_LOOP('',(#3460,#3461));
#975=EDGE_LOOP('',(#3462,#3463));
#976=EDGE_LOOP('',(#3464));
#977=EDGE_LOOP('',(#3465,#3466,#3467,#3468));
#978=EDGE_LOOP('',(#3469));
#979=EDGE_LOOP('',(#3470));
#980=EDGE_LOOP('',(#3471,#3472,#3473,#3474,#3475,#3476,#3477,#3478,#3479,
#3480,#3481,#3482,#3483,#3484,#3485,#3486,#3487,#3488,#3489));
#981=EDGE_LOOP('',(#3490));
#982=EDGE_LOOP('',(#3491));
#983=EDGE_LOOP('',(#3492));
#984=EDGE_LOOP('',(#3493));
#985=EDGE_LOOP('',(#3494));
#986=EDGE_LOOP('',(#3495));
#987=EDGE_LOOP('',(#3496,#3497));
#988=EDGE_LOOP('',(#3498,#3499));
#989=EDGE_LOOP('',(#3500,#3501));
#990=EDGE_LOOP('',(#3502));
#991=EDGE_LOOP('',(#3503));
#992=EDGE_LOOP('',(#3504));
#993=EDGE_LOOP('',(#3505));
#994=EDGE_LOOP('',(#3506));
#995=EDGE_LOOP('',(#3507,#3508,#3509,#3510));
#996=EDGE_LOOP('',(#3511));
#997=EDGE_LOOP('',(#3512,#3513,#3514,#3515));
#998=EDGE_LOOP('',(#3516));
#999=EDGE_LOOP('',(#3517,#3518,#3519,#3520));
#1000=EDGE_LOOP('',(#3521));
#1001=EDGE_LOOP('',(#3522));
#1002=EDGE_LOOP('',(#3523,#3524,#3525,#3526));
#1003=EDGE_LOOP('',(#3527,#3528,#3529,#3530));
#1004=EDGE_LOOP('',(#3531,#3532,#3533,#3534));
#1005=EDGE_LOOP('',(#3535,#3536,#3537,#3538));
#1006=EDGE_LOOP('',(#3539,#3540,#3541,#3542));
#1007=EDGE_LOOP('',(#3543,#3544,#3545,#3546,#3547));
#1008=EDGE_LOOP('',(#3548,#3549,#3550,#3551,#3552));
#1009=EDGE_LOOP('',(#3553,#3554,#3555,#3556));
#1010=EDGE_LOOP('',(#3557,#3558,#3559,#3560));
#1011=EDGE_LOOP('',(#3561,#3562,#3563,#3564));
#1012=EDGE_LOOP('',(#3565,#3566,#3567,#3568));
#1013=EDGE_LOOP('',(#3569,#3570,#3571,#3572));
#1014=EDGE_LOOP('',(#3573,#3574,#3575,#3576));
#1015=EDGE_LOOP('',(#3577,#3578,#3579,#3580));
#1016=EDGE_LOOP('',(#3581));
#1017=EDGE_LOOP('',(#3582));
#1018=EDGE_LOOP('',(#3583,#3584,#3585,#3586));
#1019=EDGE_LOOP('',(#3587));
#1020=EDGE_LOOP('',(#3588));
#1021=EDGE_LOOP('',(#3589,#3590,#3591,#3592));
#1022=EDGE_LOOP('',(#3593,#3594,#3595,#3596));
#1023=EDGE_LOOP('',(#3597,#3598,#3599,#3600));
#1024=EDGE_LOOP('',(#3601));
#1025=EDGE_LOOP('',(#3602));
#1026=EDGE_LOOP('',(#3603));
#1027=EDGE_LOOP('',(#3604));
#1028=EDGE_LOOP('',(#3605,#3606,#3607,#3608));
#1029=EDGE_LOOP('',(#3609,#3610,#3611,#3612,#3613,#3614,#3615,#3616));
#1030=EDGE_LOOP('',(#3617,#3618,#3619,#3620));
#1031=EDGE_LOOP('',(#3621,#3622,#3623,#3624,#3625,#3626,#3627,#3628));
#1032=EDGE_LOOP('',(#3629,#3630,#3631,#3632));
#1033=EDGE_LOOP('',(#3633));
#1034=EDGE_LOOP('',(#3634));
#1035=EDGE_LOOP('',(#3635));
#1036=EDGE_LOOP('',(#3636,#3637,#3638,#3639));
#1037=EDGE_LOOP('',(#3640));
#1038=EDGE_LOOP('',(#3641));
#1039=EDGE_LOOP('',(#3642));
#1040=EDGE_LOOP('',(#3643,#3644,#3645,#3646,#3647,#3648));
#1041=EDGE_LOOP('',(#3649));
#1042=EDGE_LOOP('',(#3650,#3651,#3652,#3653,#3654,#3655));
#1043=EDGE_LOOP('',(#3656));
#1044=EDGE_LOOP('',(#3657,#3658,#3659,#3660));
#1045=EDGE_LOOP('',(#3661,#3662,#3663,#3664));
#1046=EDGE_LOOP('',(#3665,#3666,#3667,#3668));
#1047=EDGE_LOOP('',(#3669,#3670,#3671,#3672));
#1048=EDGE_LOOP('',(#3673,#3674,#3675,#3676));
#1049=EDGE_LOOP('',(#3677,#3678,#3679,#3680));
#1050=EDGE_LOOP('',(#3681,#3682,#3683,#3684));
#1051=EDGE_LOOP('',(#3685));
#1052=EDGE_LOOP('',(#3686));
#1053=EDGE_LOOP('',(#3687,#3688,#3689,#3690));
#1054=EDGE_LOOP('',(#3691,#3692,#3693,#3694));
#1055=EDGE_LOOP('',(#3695,#3696,#3697,#3698));
#1056=EDGE_LOOP('',(#3699));
#1057=EDGE_LOOP('',(#3700));
#1058=EDGE_LOOP('',(#3701,#3702,#3703,#3704));
#1059=EDGE_LOOP('',(#3705,#3706,#3707,#3708));
#1060=EDGE_LOOP('',(#3709,#3710,#3711,#3712));
#1061=EDGE_LOOP('',(#3713));
#1062=EDGE_LOOP('',(#3714));
#1063=EDGE_LOOP('',(#3715));
#1064=EDGE_LOOP('',(#3716));
#1065=EDGE_LOOP('',(#3717));
#1066=EDGE_LOOP('',(#3718));
#1067=EDGE_LOOP('',(#3719,#3720,#3721,#3722));
#1068=EDGE_LOOP('',(#3723));
#1069=EDGE_LOOP('',(#3724));
#1070=EDGE_LOOP('',(#3725));
#1071=EDGE_LOOP('',(#3726));
#1072=EDGE_LOOP('',(#3727,#3728,#3729,#3730));
#1073=EDGE_LOOP('',(#3731,#3732,#3733,#3734));
#1074=EDGE_LOOP('',(#3735,#3736,#3737,#3738));
#1075=EDGE_LOOP('',(#3739));
#1076=EDGE_LOOP('',(#3740,#3741,#3742,#3743));
#1077=EDGE_LOOP('',(#3744));
#1078=EDGE_LOOP('',(#3745));
#1079=EDGE_LOOP('',(#3746));
#1080=EDGE_LOOP('',(#3747,#3748,#3749,#3750));
#1081=EDGE_LOOP('',(#3751,#3752,#3753,#3754));
#1082=EDGE_LOOP('',(#3755));
#1083=EDGE_LOOP('',(#3756));
#1084=EDGE_LOOP('',(#3757));
#1085=EDGE_LOOP('',(#3758));
#1086=EDGE_LOOP('',(#3759,#3760,#3761,#3762));
#1087=EDGE_LOOP('',(#3763,#3764,#3765,#3766));
#1088=EDGE_LOOP('',(#3767,#3768,#3769,#3770));
#1089=EDGE_LOOP('',(#3771,#3772,#3773,#3774));
#1090=EDGE_LOOP('',(#3775,#3776,#3777,#3778));
#1091=EDGE_LOOP('',(#3779,#3780,#3781,#3782));
#1092=EDGE_LOOP('',(#3783,#3784,#3785,#3786));
#1093=EDGE_LOOP('',(#3787,#3788,#3789,#3790));
#1094=EDGE_LOOP('',(#3791));
#1095=EDGE_LOOP('',(#3792));
#1096=EDGE_LOOP('',(#3793));
#1097=EDGE_LOOP('',(#3794));
#1098=EDGE_LOOP('',(#3795));
#1099=EDGE_LOOP('',(#3796));
#1100=EDGE_LOOP('',(#3797));
#1101=EDGE_LOOP('',(#3798));
#1102=EDGE_LOOP('',(#3799));
#1103=EDGE_LOOP('',(#3800));
#1104=EDGE_LOOP('',(#3801));
#1105=EDGE_LOOP('',(#3802));
#1106=EDGE_LOOP('',(#3803));
#1107=EDGE_LOOP('',(#3804));
#1108=EDGE_LOOP('',(#3805));
#1109=EDGE_LOOP('',(#3806));
#1110=EDGE_LOOP('',(#3807,#3808,#3809,#3810));
#1111=EDGE_LOOP('',(#3811,#3812,#3813,#3814));
#1112=EDGE_LOOP('',(#3815));
#1113=EDGE_LOOP('',(#3816));
#1114=EDGE_LOOP('',(#3817));
#1115=EDGE_LOOP('',(#3818));
#1116=EDGE_LOOP('',(#3819,#3820,#3821,#3822));
#1117=EDGE_LOOP('',(#3823,#3824,#3825,#3826));
#1118=EDGE_LOOP('',(#3827));
#1119=EDGE_LOOP('',(#3828));
#1120=EDGE_LOOP('',(#3829));
#1121=EDGE_LOOP('',(#3830));
#1122=EDGE_LOOP('',(#3831,#3832));
#1123=EDGE_LOOP('',(#3833,#3834,#3835,#3836));
#1124=EDGE_LOOP('',(#3837,#3838,#3839,#3840));
#1125=EDGE_LOOP('',(#3841,#3842));
#1126=EDGE_LOOP('',(#3843,#3844));
#1127=EDGE_LOOP('',(#3845,#3846,#3847,#3848));
#1128=EDGE_LOOP('',(#3849,#3850));
#1129=EDGE_LOOP('',(#3851,#3852,#3853,#3854));
#1130=EDGE_LOOP('',(#3855,#3856));
#1131=EDGE_LOOP('',(#3857,#3858,#3859,#3860));
#1132=EDGE_LOOP('',(#3861,#3862,#3863,#3864));
#1133=EDGE_LOOP('',(#3865,#3866));
#1134=EDGE_LOOP('',(#3867,#3868,#3869,#3870,#3871,#3872,#3873,#3874,#3875,
#3876,#3877,#3878,#3879,#3880,#3881,#3882,#3883,#3884,#3885,#3886,#3887,
#3888,#3889,#3890,#3891,#3892,#3893,#3894));
#1135=EDGE_LOOP('',(#3895,#3896,#3897,#3898));
#1136=EDGE_LOOP('',(#3899,#3900,#3901,#3902));
#1137=EDGE_LOOP('',(#3903,#3904,#3905,#3906));
#1138=EDGE_LOOP('',(#3907,#3908,#3909,#3910));
#1139=EDGE_LOOP('',(#3911,#3912,#3913,#3914));
#1140=EDGE_LOOP('',(#3915,#3916,#3917,#3918));
#1141=EDGE_LOOP('',(#3919,#3920,#3921,#3922));
#1142=EDGE_LOOP('',(#3923,#3924,#3925,#3926));
#1143=EDGE_LOOP('',(#3927));
#1144=EDGE_LOOP('',(#3928));
#1145=EDGE_LOOP('',(#3929));
#1146=EDGE_LOOP('',(#3930));
#1147=EDGE_LOOP('',(#3931,#3932,#3933,#3934));
#1148=EDGE_LOOP('',(#3935));
#1149=EDGE_LOOP('',(#3936));
#1150=EDGE_LOOP('',(#3937));
#1151=EDGE_LOOP('',(#3938));
#1152=EDGE_LOOP('',(#3939));
#1153=EDGE_LOOP('',(#3940));
#1154=EDGE_LOOP('',(#3941));
#1155=EDGE_LOOP('',(#3942,#3943,#3944,#3945,#3946,#3947,#3948,#3949,#3950,
#3951,#3952,#3953,#3954));
#1156=EDGE_LOOP('',(#3955));
#1157=EDGE_LOOP('',(#3956));
#1158=EDGE_LOOP('',(#3957));
#1159=EDGE_LOOP('',(#3958));
#1160=EDGE_LOOP('',(#3959));
#1161=EDGE_LOOP('',(#3960));
#1162=EDGE_LOOP('',(#3961));
#1163=EDGE_LOOP('',(#3962));
#1164=EDGE_LOOP('',(#3963,#3964,#3965,#3966));
#1165=EDGE_LOOP('',(#3967));
#1166=EDGE_LOOP('',(#3968));
#1167=EDGE_LOOP('',(#3969,#3970,#3971,#3972));
#1168=EDGE_LOOP('',(#3973));
#1169=EDGE_LOOP('',(#3974,#3975,#3976,#3977));
#1170=EDGE_LOOP('',(#3978));
#1171=EDGE_LOOP('',(#3979));
#1172=EDGE_LOOP('',(#3980));
#1173=EDGE_LOOP('',(#3981,#3982,#3983,#3984));
#1174=EDGE_LOOP('',(#3985));
#1175=EDGE_LOOP('',(#3986));
#1176=EDGE_LOOP('',(#3987,#3988,#3989));
#1177=EDGE_LOOP('',(#3990,#3991,#3992,#3993,#3994,#3995,#3996,#3997));
#1178=EDGE_LOOP('',(#3998,#3999));
#1179=EDGE_LOOP('',(#4000,#4001,#4002,#4003));
#1180=EDGE_LOOP('',(#4004,#4005,#4006,#4007));
#1181=EDGE_LOOP('',(#4008,#4009,#4010,#4011));
#1182=EDGE_LOOP('',(#4012));
#1183=EDGE_LOOP('',(#4013));
#1184=EDGE_LOOP('',(#4014));
#1185=EDGE_LOOP('',(#4015));
#1186=EDGE_LOOP('',(#4016));
#1187=EDGE_LOOP('',(#4017));
#1188=EDGE_LOOP('',(#4018,#4019,#4020,#4021));
#1189=EDGE_LOOP('',(#4022,#4023,#4024,#4025));
#1190=EDGE_LOOP('',(#4026,#4027,#4028,#4029));
#1191=EDGE_LOOP('',(#4030));
#1192=EDGE_LOOP('',(#4031));
#1193=EDGE_LOOP('',(#4032,#4033,#4034,#4035));
#1194=EDGE_LOOP('',(#4036,#4037,#4038,#4039));
#1195=EDGE_LOOP('',(#4040,#4041,#4042,#4043));
#1196=EDGE_LOOP('',(#4044));
#1197=EDGE_LOOP('',(#4045,#4046,#4047,#4048));
#1198=EDGE_LOOP('',(#4049,#4050,#4051,#4052));
#1199=EDGE_LOOP('',(#4053,#4054,#4055,#4056));
#1200=EDGE_LOOP('',(#4057,#4058,#4059,#4060));
#1201=EDGE_LOOP('',(#4061,#4062,#4063,#4064));
#1202=EDGE_LOOP('',(#4065,#4066,#4067,#4068));
#1203=EDGE_LOOP('',(#4069,#4070,#4071,#4072,#4073,#4074));
#1204=EDGE_LOOP('',(#4075,#4076,#4077,#4078,#4079,#4080));
#1205=EDGE_LOOP('',(#4081,#4082,#4083,#4084));
#1206=EDGE_LOOP('',(#4085,#4086,#4087,#4088));
#1207=EDGE_LOOP('',(#4089));
#1208=EDGE_LOOP('',(#4090));
#1209=EDGE_LOOP('',(#4091));
#1210=EDGE_LOOP('',(#4092));
#1211=EDGE_LOOP('',(#4093,#4094,#4095,#4096,#4097,#4098,#4099,#4100,#4101));
#1212=EDGE_LOOP('',(#4102,#4103,#4104,#4105,#4106,#4107,#4108,#4109,#4110));
#1213=EDGE_LOOP('',(#4111,#4112,#4113,#4114));
#1214=EDGE_LOOP('',(#4115,#4116,#4117,#4118));
#1215=EDGE_LOOP('',(#4119,#4120,#4121,#4122));
#1216=EDGE_LOOP('',(#4123,#4124,#4125,#4126));
#1217=EDGE_LOOP('',(#4127,#4128,#4129,#4130));
#1218=EDGE_LOOP('',(#4131,#4132,#4133,#4134));
#1219=EDGE_LOOP('',(#4135,#4136,#4137,#4138));
#1220=EDGE_LOOP('',(#4139));
#1221=EDGE_LOOP('',(#4140));
#1222=EDGE_LOOP('',(#4141));
#1223=EDGE_LOOP('',(#4142));
#1224=EDGE_LOOP('',(#4143,#4144,#4145,#4146));
#1225=EDGE_LOOP('',(#4147,#4148,#4149,#4150));
#1226=EDGE_LOOP('',(#4151,#4152,#4153,#4154));
#1227=EDGE_LOOP('',(#4155,#4156,#4157,#4158));
#1228=EDGE_LOOP('',(#4159,#4160,#4161,#4162));
#1229=EDGE_LOOP('',(#4163,#4164,#4165,#4166));
#1230=EDGE_LOOP('',(#4167,#4168,#4169,#4170,#4171,#4172));
#1231=EDGE_LOOP('',(#4173));
#1232=EDGE_LOOP('',(#4174,#4175,#4176,#4177,#4178,#4179));
#1233=EDGE_LOOP('',(#4180,#4181,#4182,#4183));
#1234=EDGE_LOOP('',(#4184,#4185,#4186,#4187));
#1235=EDGE_LOOP('',(#4188,#4189,#4190,#4191));
#1236=EDGE_LOOP('',(#4192));
#1237=EDGE_LOOP('',(#4193,#4194,#4195,#4196));
#1238=EDGE_LOOP('',(#4197,#4198,#4199,#4200));
#1239=EDGE_LOOP('',(#4201,#4202,#4203,#4204));
#1240=EDGE_LOOP('',(#4205,#4206,#4207,#4208));
#1241=EDGE_LOOP('',(#4209,#4210,#4211,#4212));
#1242=EDGE_LOOP('',(#4213,#4214,#4215,#4216));
#1243=EDGE_LOOP('',(#4217,#4218,#4219,#4220));
#1244=EDGE_LOOP('',(#4221));
#1245=EDGE_LOOP('',(#4222,#4223,#4224,#4225));
#1246=EDGE_LOOP('',(#4226));
#1247=EDGE_LOOP('',(#4227));
#1248=EDGE_LOOP('',(#4228,#4229,#4230,#4231));
#1249=EDGE_LOOP('',(#4232,#4233,#4234,#4235));
#1250=EDGE_LOOP('',(#4236,#4237,#4238,#4239));
#1251=EDGE_LOOP('',(#4240));
#1252=EDGE_LOOP('',(#4241));
#1253=EDGE_LOOP('',(#4242,#4243,#4244,#4245));
#1254=EDGE_LOOP('',(#4246,#4247,#4248,#4249));
#1255=EDGE_LOOP('',(#4250,#4251,#4252,#4253));
#1256=EDGE_LOOP('',(#4254));
#1257=EDGE_LOOP('',(#4255,#4256,#4257,#4258));
#1258=EDGE_LOOP('',(#4259,#4260,#4261,#4262));
#1259=EDGE_LOOP('',(#4263,#4264,#4265,#4266));
#1260=EDGE_LOOP('',(#4267,#4268,#4269,#4270));
#1261=EDGE_LOOP('',(#4271,#4272,#4273,#4274));
#1262=EDGE_LOOP('',(#4275,#4276,#4277,#4278));
#1263=EDGE_LOOP('',(#4279,#4280,#4281,#4282,#4283,#4284));
#1264=EDGE_LOOP('',(#4285,#4286,#4287,#4288,#4289,#4290));
#1265=B_SPLINE_CURVE_WITH_KNOTS('',3,(#7016,#7017,#7018,#7019,#7020,#7021,
#7022,#7023,#7024,#7025),.UNSPECIFIED.,.F.,.F.,(4,2,2,2,4),(0.,0.0624222198205065,
0.124844439641013,0.187259170559066,0.249673901477119),.UNSPECIFIED.);
#1266=B_SPLINE_CURVE_WITH_KNOTS('',3,(#7026,#7027,#7028,#7029,#7030,#7031,
#7032,#7033,#7034,#7035,#7036,#7037,#7038,#7039,#7040,#7041,#7042,#7043,
#7044,#7045,#7046,#7047,#7048,#7049,#7050,#7051),.UNSPECIFIED.,.F.,.F.,
(4,2,2,2,2,2,2,2,2,2,2,2,4),(0.249673901477119,0.312088632395172,0.374503363313225,
0.436925583133731,0.499347802954238,0.561770022774744,0.624192242595251,
0.686606973513304,0.749021704431357,0.811436435349409,0.873851166267462,
0.936273386087969,0.998695605908476),.UNSPECIFIED.);
#1267=B_SPLINE_CURVE_WITH_KNOTS('',3,(#7114,#7115,#7116,#7117,#7118,#7119,
#7120,#7121,#7122,#7123,#7124,#7125,#7126,#7127),.UNSPECIFIED.,.F.,.F.,
(4,2,2,2,2,2,4),(0.737404739505917,0.796636749554485,0.876284832373894,
0.955932915193303,1.03558099801271,1.11522908083212,1.17446109088069),
 .UNSPECIFIED.);
#1268=B_SPLINE_CURVE_WITH_KNOTS('',3,(#7201,#7202,#7203,#7204,#7205,#7206,
#7207,#7208,#7209,#7210,#7211,#7212,#7213,#7214,#7215,#7216,#7217,#7218,
#7219,#7220,#7221,#7222,#7223,#7224,#7225,#7226,#7227,#7228,#7229,#7230,
#7231,#7232,#7233,#7234),.UNSPECIFIED.,.T.,.F.,(4,2,2,2,2,2,2,2,2,2,2,2,
2,2,2,2,4),(0.,0.0759876362447374,0.151975272489475,0.227927665609886,0.303880058730296,
0.379832451850707,0.455784844971118,0.531772481215856,0.607760117460593,
0.68374775370533,0.759735389950068,0.835687783070479,0.911640176190889,
0.9875925693113,1.06354496243171,1.13953259867645,1.21552023492119),
 .UNSPECIFIED.);
#1269=B_SPLINE_CURVE_WITH_KNOTS('',3,(#7237,#7238,#7239,#7240,#7241,#7242,
#7243,#7244,#7245,#7246,#7247,#7248,#7249,#7250,#7251,#7252,#7253,#7254,
#7255,#7256,#7257,#7258,#7259,#7260,#7261,#7262,#7263,#7264,#7265,#7266,
#7267,#7268,#7269,#7270),.UNSPECIFIED.,.T.,.F.,(4,2,2,2,2,2,2,2,2,2,2,2,
2,2,2,2,4),(0.,0.258464867281583,0.516929734563166,0.775389819140497,1.03384990371783,
1.29230998829516,1.55077007287249,1.80923494015407,2.06769980743566,2.32616467471724,
2.58462954199882,2.84308962657615,3.10154971115348,3.36000979573081,3.61846988030814,
3.87693474758973,4.13539961487131),.UNSPECIFIED.);
#1270=B_SPLINE_CURVE_WITH_KNOTS('',3,(#7275,#7276,#7277,#7278,#7279,#7280,
#7281,#7282,#7283,#7284),.UNSPECIFIED.,.F.,.F.,(4,2,2,2,4),(0.,0.150955476673376,
0.301910953346751,0.452863012665493,0.603815071984235),.UNSPECIFIED.);
#1271=B_SPLINE_CURVE_WITH_KNOTS('',3,(#7285,#7286,#7287,#7288,#7289,#7290,
#7291,#7292,#7293,#7294,#7295,#7296,#7297,#7298,#7299,#7300,#7301,#7302,
#7303,#7304,#7305,#7306,#7307,#7308,#7309,#7310),.UNSPECIFIED.,.F.,.F.,
(4,2,2,2,2,2,2,2,2,2,2,2,4),(0.603815071984235,0.754767131302978,0.90571919062172,
1.0566746672951,1.20763014396847,1.35858562064185,1.50954109731522,1.66049315663396,
1.81144521595271,1.96239727527145,2.11334933459019,2.26430481126357,2.41526028793694),
 .UNSPECIFIED.);
#1272=B_SPLINE_CURVE_WITH_KNOTS('',3,(#7320,#7321,#7322,#7323,#7324,#7325,
#7326,#7327,#7328,#7329,#7330,#7331,#7332,#7333,#7334,#7335,#7336,#7337,
#7338,#7339,#7340,#7341,#7342,#7343,#7344,#7345),.UNSPECIFIED.,.F.,.F.,
(4,2,2,2,2,2,2,2,2,2,2,2,4),(0.,0.258464867281583,0.516929734563165,0.775389819140496,
1.03384990371783,1.29230998829516,1.55077007287249,1.80923494015407,2.06769980743565,
2.32616467471724,2.58462954199882,2.84308962657615,3.10154971115348),
 .UNSPECIFIED.);
#1273=B_SPLINE_CURVE_WITH_KNOTS('',3,(#7346,#7347,#7348,#7349,#7350,#7351,
#7352,#7353,#7354,#7355),.UNSPECIFIED.,.F.,.F.,(4,2,2,2,4),(3.10154971115348,
3.36000979573081,3.61846988030814,3.87693474758973,4.13539961487131),
 .UNSPECIFIED.);
#1274=B_SPLINE_CURVE_WITH_KNOTS('',3,(#7404,#7405,#7406,#7407,#7408,#7409,
#7410,#7411,#7412,#7413),.UNSPECIFIED.,.F.,.F.,(4,2,2,2,4),(0.,0.258464867281583,
0.516929734563165,0.775389819140497,1.03384990371783),.UNSPECIFIED.);
#1275=B_SPLINE_CURVE_WITH_KNOTS('',3,(#7415,#7416,#7417,#7418,#7419,#7420,
#7421,#7422,#7423,#7424),.UNSPECIFIED.,.F.,.F.,(4,2,2,2,4),(3.10154971115348,
3.36000979573081,3.61846988030815,3.87693474758973,4.13539961487131),
 .UNSPECIFIED.);
#1276=B_SPLINE_CURVE_WITH_KNOTS('',3,(#7425,#7426,#7427,#7428,#7429,#7430,
#7431,#7432,#7433,#7434,#7435,#7436,#7437,#7438,#7439,#7440,#7441,#7442),
 .UNSPECIFIED.,.F.,.F.,(4,2,2,2,2,2,2,2,4),(1.03384990371783,1.29230998829516,
1.55077007287249,1.80923494015407,2.06769980743566,2.32616467471724,2.58462954199882,
2.84308962657615,3.10154971115348),.UNSPECIFIED.);
#1277=B_SPLINE_CURVE_WITH_KNOTS('',3,(#7517,#7518,#7519,#7520,#7521,#7522,
#7523,#7524,#7525,#7526,#7527,#7528,#7529,#7530,#7531,#7532,#7533,#7534,
#7535,#7536,#7537,#7538,#7539,#7540,#7541,#7542,#7543,#7544,#7545,#7546,
#7547,#7548,#7549,#7550),.UNSPECIFIED.,.T.,.F.,(4,2,2,2,2,2,2,2,2,2,2,2,
2,2,2,2,4),(0.,0.0188366744349197,0.0376733488698393,0.0565100213871705,
0.0753466939045016,0.0941833664218328,0.113020038939164,0.131856713374084,
0.150693387809003,0.169530062243923,0.188366736678843,0.207203409196174,
0.226040081713505,0.244876754230836,0.263713426748167,0.282550101183087,
0.301386775618006),.UNSPECIFIED.);
#1278=B_SPLINE_CURVE_WITH_KNOTS('',3,(#7553,#7554,#7555,#7556,#7557,#7558,
#7559,#7560,#7561,#7562,#7563,#7564,#7565,#7566,#7567,#7568,#7569,#7570,
#7571,#7572,#7573,#7574,#7575,#7576,#7577,#7578,#7579,#7580,#7581,#7582,
#7583,#7584,#7585,#7586),.UNSPECIFIED.,.T.,.F.,(4,2,2,2,2,2,2,2,2,2,2,2,
2,2,2,2,4),(0.,0.0188556028927646,0.0377112057855292,0.0565666511569687,
0.0754220965284081,0.0942775418998475,0.113132987271287,0.131988590164052,
0.150844193056816,0.169699795949581,0.188555398842345,0.207410844213785,
0.226266289585224,0.245121734956664,0.263977180328103,0.282832783220868,
0.301688386113632),.UNSPECIFIED.);
#1279=B_SPLINE_CURVE_WITH_KNOTS('',3,(#7589,#7590,#7591,#7592,#7593,#7594,
#7595,#7596,#7597,#7598,#7599,#7600,#7601,#7602,#7603,#7604,#7605,#7606,
#7607,#7608,#7609,#7610,#7611,#7612,#7613,#7614,#7615,#7616,#7617,#7618,
#7619,#7620,#7621,#7622),.UNSPECIFIED.,.T.,.F.,(4,2,2,2,2,2,2,2,2,2,2,2,
2,2,2,2,4),(0.,0.0188556028927646,0.0377112057855292,0.0565666511569687,
0.0754220965284081,0.0942775418998475,0.113132987271287,0.131988590164052,
0.150844193056816,0.169699795949581,0.188555398842345,0.207410844213785,
0.226266289585224,0.245121734956664,0.263977180328103,0.282832783220868,
0.301688386113632),.UNSPECIFIED.);
#1280=B_SPLINE_CURVE_WITH_KNOTS('',3,(#7625,#7626,#7627,#7628,#7629,#7630,
#7631,#7632,#7633,#7634,#7635,#7636,#7637,#7638,#7639,#7640,#7641,#7642,
#7643,#7644,#7645,#7646,#7647,#7648,#7649,#7650,#7651,#7652,#7653,#7654,
#7655,#7656,#7657,#7658),.UNSPECIFIED.,.T.,.F.,(4,2,2,2,2,2,2,2,2,2,2,2,
2,2,2,2,4),(0.,0.0188366744349197,0.0376733488698393,0.0565100213871705,
0.0753466939045016,0.0941833664218328,0.113020038939164,0.131856713374084,
0.150693387809003,0.169530062243923,0.188366736678843,0.207203409196174,
0.226040081713505,0.244876754230836,0.263713426748167,0.282550101183087,
0.301386775618006),.UNSPECIFIED.);
#1281=B_SPLINE_CURVE_WITH_KNOTS('',3,(#7661,#7662,#7663,#7664,#7665,#7666,
#7667,#7668,#7669,#7670,#7671,#7672,#7673,#7674,#7675,#7676,#7677,#7678,
#7679,#7680,#7681,#7682,#7683,#7684,#7685,#7686,#7687,#7688,#7689,#7690,
#7691,#7692,#7693,#7694),.UNSPECIFIED.,.T.,.F.,(4,2,2,2,2,2,2,2,2,2,2,2,
2,2,2,2,4),(0.,0.0188366744349197,0.0376733488698393,0.0565100213871705,
0.0753466939045016,0.0941833664218328,0.113020038939164,0.131856713374084,
0.150693387809003,0.169530062243923,0.188366736678843,0.207203409196174,
0.226040081713505,0.244876754230836,0.263713426748167,0.282550101183087,
0.301386775618007),.UNSPECIFIED.);
#1282=B_SPLINE_CURVE_WITH_KNOTS('',3,(#7697,#7698,#7699,#7700,#7701,#7702,
#7703,#7704,#7705,#7706,#7707,#7708,#7709,#7710,#7711,#7712,#7713,#7714,
#7715,#7716,#7717,#7718,#7719,#7720,#7721,#7722,#7723,#7724,#7725,#7726,
#7727,#7728,#7729,#7730),.UNSPECIFIED.,.T.,.F.,(4,2,2,2,2,2,2,2,2,2,2,2,
2,2,2,2,4),(0.,0.0188556028927646,0.0377112057855293,0.0565666511569687,
0.0754220965284081,0.0942775418998476,0.113132987271287,0.131988590164052,
0.150844193056816,0.169699795949581,0.188555398842346,0.207410844213785,
0.226266289585224,0.245121734956664,0.263977180328103,0.282832783220868,
0.301688386113632),.UNSPECIFIED.);
#1283=B_SPLINE_CURVE_WITH_KNOTS('',3,(#7733,#7734,#7735,#7736,#7737,#7738,
#7739,#7740,#7741,#7742,#7743,#7744,#7745,#7746,#7747,#7748,#7749,#7750,
#7751,#7752,#7753,#7754,#7755,#7756,#7757,#7758,#7759,#7760,#7761,#7762,
#7763,#7764,#7765,#7766),.UNSPECIFIED.,.T.,.F.,(4,2,2,2,2,2,2,2,2,2,2,2,
2,2,2,2,4),(0.,0.0188556028927646,0.0377112057855292,0.0565666511569687,
0.0754220965284081,0.0942775418998475,0.113132987271287,0.131988590164052,
0.150844193056816,0.169699795949581,0.188555398842345,0.207410844213785,
0.226266289585224,0.245121734956664,0.263977180328103,0.282832783220868,
0.301688386113632),.UNSPECIFIED.);
#1284=B_SPLINE_CURVE_WITH_KNOTS('',3,(#7769,#7770,#7771,#7772,#7773,#7774,
#7775,#7776,#7777,#7778,#7779,#7780,#7781,#7782,#7783,#7784,#7785,#7786,
#7787,#7788,#7789,#7790,#7791,#7792,#7793,#7794,#7795,#7796,#7797,#7798,
#7799,#7800,#7801,#7802),.UNSPECIFIED.,.T.,.F.,(4,2,2,2,2,2,2,2,2,2,2,2,
2,2,2,2,4),(0.,0.0188366744349198,0.0376733488698396,0.0565100213871707,
0.0753466939045018,0.094183366421833,0.113020038939164,0.131856713374084,
0.150693387809003,0.169530062243923,0.188366736678843,0.207203409196174,
0.226040081713505,0.244876754230836,0.263713426748167,0.282550101183087,
0.301386775618007),.UNSPECIFIED.);
#1285=B_SPLINE_CURVE_WITH_KNOTS('',3,(#7805,#7806,#7807,#7808,#7809,#7810,
#7811,#7812,#7813,#7814,#7815,#7816,#7817,#7818,#7819,#7820,#7821,#7822,
#7823,#7824,#7825,#7826,#7827,#7828,#7829,#7830,#7831,#7832,#7833,#7834,
#7835,#7836,#7837,#7838),.UNSPECIFIED.,.T.,.F.,(4,2,2,2,2,2,2,2,2,2,2,2,
2,2,2,2,4),(0.,0.0188366744349197,0.0376733488698393,0.0565100213871705,
0.0753466939045016,0.0941833664218328,0.113020038939164,0.131856713374084,
0.150693387809003,0.169530062243923,0.188366736678842,0.207203409196173,
0.226040081713505,0.244876754230836,0.263713426748167,0.282550101183086,
0.301386775618006),.UNSPECIFIED.);
#1286=B_SPLINE_CURVE_WITH_KNOTS('',3,(#7841,#7842,#7843,#7844,#7845,#7846,
#7847,#7848,#7849,#7850,#7851,#7852,#7853,#7854,#7855,#7856,#7857,#7858,
#7859,#7860,#7861,#7862,#7863,#7864,#7865,#7866,#7867,#7868,#7869,#7870,
#7871,#7872,#7873,#7874),.UNSPECIFIED.,.T.,.F.,(4,2,2,2,2,2,2,2,2,2,2,2,
2,2,2,2,4),(0.,0.0188556028927646,0.0377112057855292,0.0565666511569687,
0.0754220965284081,0.0942775418998475,0.113132987271287,0.131988590164052,
0.150844193056816,0.169699795949581,0.188555398842345,0.207410844213785,
0.226266289585224,0.245121734956664,0.263977180328103,0.282832783220868,
0.301688386113632),.UNSPECIFIED.);
#1287=B_SPLINE_CURVE_WITH_KNOTS('',3,(#7877,#7878,#7879,#7880,#7881,#7882,
#7883,#7884,#7885,#7886,#7887,#7888,#7889,#7890,#7891,#7892,#7893,#7894,
#7895,#7896,#7897,#7898,#7899,#7900,#7901,#7902,#7903,#7904,#7905,#7906,
#7907,#7908,#7909,#7910),.UNSPECIFIED.,.T.,.F.,(4,2,2,2,2,2,2,2,2,2,2,2,
2,2,2,2,4),(0.,0.0188556028927646,0.0377112057855292,0.0565666511569687,
0.0754220965284081,0.0942775418998475,0.113132987271287,0.131988590164052,
0.150844193056816,0.169699795949581,0.188555398842345,0.207410844213785,
0.226266289585224,0.245121734956664,0.263977180328103,0.282832783220868,
0.301688386113632),.UNSPECIFIED.);
#1288=B_SPLINE_CURVE_WITH_KNOTS('',3,(#7913,#7914,#7915,#7916,#7917,#7918,
#7919,#7920,#7921,#7922,#7923,#7924,#7925,#7926,#7927,#7928,#7929,#7930,
#7931,#7932,#7933,#7934,#7935,#7936,#7937,#7938,#7939,#7940,#7941,#7942,
#7943,#7944,#7945,#7946),.UNSPECIFIED.,.T.,.F.,(4,2,2,2,2,2,2,2,2,2,2,2,
2,2,2,2,4),(0.,0.0188366744349194,0.0376733488698389,0.0565100213871701,
0.0753466939045014,0.0941833664218326,0.113020038939164,0.131856713374083,
0.150693387809003,0.169530062243922,0.188366736678842,0.207203409196173,
0.226040081713504,0.244876754230835,0.263713426748167,0.282550101183086,
0.301386775618006),.UNSPECIFIED.);
#1289=B_SPLINE_CURVE_WITH_KNOTS('',3,(#7950,#7951,#7952,#7953,#7954,#7955,
#7956,#7957,#7958,#7959),.UNSPECIFIED.,.F.,.F.,(4,2,2,2,4),(0.,0.0188366744349197,
0.0376733488698393,0.0565100213871704,0.0753466939045014),.UNSPECIFIED.);
#1290=B_SPLINE_CURVE_WITH_KNOTS('',3,(#7961,#7962,#7963,#7964,#7965,#7966,
#7967,#7968,#7969,#7970),.UNSPECIFIED.,.F.,.F.,(4,2,2,2,4),(0.226040081713504,
0.244876754230835,0.263713426748166,0.282550101183086,0.301386775618006),
 .UNSPECIFIED.);
#1291=B_SPLINE_CURVE_WITH_KNOTS('',3,(#7971,#7972,#7973,#7974,#7975,#7976,
#7977,#7978,#7979,#7980,#7981,#7982,#7983,#7984,#7985,#7986,#7987,#7988),
 .UNSPECIFIED.,.F.,.F.,(4,2,2,2,2,2,2,2,4),(0.0753466939045014,0.0941833664218325,
0.113020038939164,0.131856713374083,0.150693387809003,0.169530062243923,
0.188366736678842,0.207203409196173,0.226040081713504),.UNSPECIFIED.);
#1292=B_SPLINE_CURVE_WITH_KNOTS('',3,(#7992,#7993,#7994,#7995,#7996,#7997,
#7998,#7999,#8000,#8001,#8002,#8003,#8004,#8005,#8006,#8007,#8008,#8009),
 .UNSPECIFIED.,.F.,.F.,(4,2,2,2,2,2,2,2,4),(0.0754220965284079,0.0942775418998473,
0.113132987271287,0.131988590164051,0.150844193056816,0.16969979594958,
0.188555398842345,0.207410844213784,0.226266289585224),.UNSPECIFIED.);
#1293=B_SPLINE_CURVE_WITH_KNOTS('',3,(#8011,#8012,#8013,#8014,#8015,#8016,
#8017,#8018,#8019,#8020),.UNSPECIFIED.,.F.,.F.,(4,2,2,2,4),(0.,0.0188556028927646,
0.0377112057855293,0.0565666511569686,0.0754220965284079),.UNSPECIFIED.);
#1294=B_SPLINE_CURVE_WITH_KNOTS('',3,(#8021,#8022,#8023,#8024,#8025,#8026,
#8027,#8028,#8029,#8030),.UNSPECIFIED.,.F.,.F.,(4,2,2,2,4),(0.226266289585224,
0.245121734956663,0.263977180328102,0.282832783220867,0.301688386113632),
 .UNSPECIFIED.);
#1295=B_SPLINE_CURVE_WITH_KNOTS('',3,(#8034,#8035,#8036,#8037,#8038,#8039,
#8040,#8041,#8042,#8043),.UNSPECIFIED.,.F.,.F.,(4,2,2,2,4),(0.,0.0188556028927646,
0.0377112057855293,0.0565666511569686,0.0754220965284079),.UNSPECIFIED.);
#1296=B_SPLINE_CURVE_WITH_KNOTS('',3,(#8044,#8045,#8046,#8047,#8048,#8049,
#8050,#8051,#8052,#8053,#8054,#8055,#8056,#8057,#8058,#8059,#8060,#8061,
#8062,#8063,#8064,#8065,#8066,#8067,#8068,#8069),.UNSPECIFIED.,.F.,.F.,
(4,2,2,2,2,2,2,2,2,2,2,2,4),(0.0754220965284079,0.0942775418998473,0.113132987271287,
0.131988590164051,0.150844193056816,0.16969979594958,0.188555398842345,
0.207410844213784,0.226266289585224,0.245121734956663,0.263977180328102,
0.282832783220867,0.301688386113632),.UNSPECIFIED.);
#1297=B_SPLINE_CURVE_WITH_KNOTS('',3,(#8073,#8074,#8075,#8076,#8077,#8078,
#8079,#8080,#8081,#8082,#8083,#8084,#8085,#8086,#8087,#8088,#8089,#8090,
#8091,#8092,#8093,#8094,#8095,#8096,#8097,#8098),.UNSPECIFIED.,.F.,.F.,
(4,2,2,2,2,2,2,2,2,2,2,2,4),(0.,0.0188366744349197,0.0376733488698393,0.0565100213871704,
0.0753466939045015,0.0941833664218325,0.113020038939164,0.131856713374083,
0.150693387809003,0.169530062243923,0.188366736678842,0.207203409196173,
0.226040081713504),.UNSPECIFIED.);
#1298=B_SPLINE_CURVE_WITH_KNOTS('',3,(#8099,#8100,#8101,#8102,#8103,#8104,
#8105,#8106,#8107,#8108),.UNSPECIFIED.,.F.,.F.,(4,2,2,2,4),(0.226040081713504,
0.244876754230835,0.263713426748167,0.282550101183086,0.301386775618006),
 .UNSPECIFIED.);
#1299=B_SPLINE_CURVE_WITH_KNOTS('',3,(#8112,#8113,#8114,#8115,#8116,#8117,
#8118,#8119,#8120,#8121),.UNSPECIFIED.,.F.,.F.,(4,2,2,2,4),(0.,0.0188366744349197,
0.0376733488698393,0.0565100213871705,0.0753466939045016),.UNSPECIFIED.);
#1300=B_SPLINE_CURVE_WITH_KNOTS('',3,(#8123,#8124,#8125,#8126,#8127,#8128,
#8129,#8130,#8131,#8132),.UNSPECIFIED.,.F.,.F.,(4,2,2,2,4),(0.226040081713505,
0.244876754230836,0.263713426748167,0.282550101183087,0.301386775618007),
 .UNSPECIFIED.);
#1301=B_SPLINE_CURVE_WITH_KNOTS('',3,(#8133,#8134,#8135,#8136,#8137,#8138,
#8139,#8140,#8141,#8142,#8143,#8144,#8145,#8146,#8147,#8148,#8149,#8150),
 .UNSPECIFIED.,.F.,.F.,(4,2,2,2,2,2,2,2,4),(0.0753466939045016,0.0941833664218328,
0.113020038939164,0.131856713374084,0.150693387809003,0.169530062243923,
0.188366736678843,0.207203409196174,0.226040081713505),.UNSPECIFIED.);
#1302=B_SPLINE_CURVE_WITH_KNOTS('',3,(#8154,#8155,#8156,#8157,#8158,#8159,
#8160,#8161,#8162,#8163,#8164,#8165,#8166,#8167,#8168,#8169,#8170,#8171),
 .UNSPECIFIED.,.F.,.F.,(4,2,2,2,2,2,2,2,4),(0.0754220965284082,0.0942775418998476,
0.113132987271287,0.131988590164052,0.150844193056816,0.169699795949581,
0.188555398842346,0.207410844213785,0.226266289585224),.UNSPECIFIED.);
#1303=B_SPLINE_CURVE_WITH_KNOTS('',3,(#8173,#8174,#8175,#8176,#8177,#8178,
#8179,#8180,#8181,#8182),.UNSPECIFIED.,.F.,.F.,(4,2,2,2,4),(0.,0.0188556028927646,
0.0377112057855293,0.0565666511569687,0.0754220965284082),.UNSPECIFIED.);
#1304=B_SPLINE_CURVE_WITH_KNOTS('',3,(#8183,#8184,#8185,#8186,#8187,#8188,
#8189,#8190,#8191,#8192),.UNSPECIFIED.,.F.,.F.,(4,2,2,2,4),(0.226266289585224,
0.245121734956664,0.263977180328103,0.282832783220868,0.301688386113633),
 .UNSPECIFIED.);
#1305=B_SPLINE_CURVE_WITH_KNOTS('',3,(#8196,#8197,#8198,#8199,#8200,#8201,
#8202,#8203,#8204,#8205),.UNSPECIFIED.,.F.,.F.,(4,2,2,2,4),(0.,0.0188556028927646,
0.0377112057855293,0.0565666511569687,0.0754220965284081),.UNSPECIFIED.);
#1306=B_SPLINE_CURVE_WITH_KNOTS('',3,(#8206,#8207,#8208,#8209,#8210,#8211,
#8212,#8213,#8214,#8215,#8216,#8217,#8218,#8219,#8220,#8221,#8222,#8223,
#8224,#8225,#8226,#8227,#8228,#8229,#8230,#8231),.UNSPECIFIED.,.F.,.F.,
(4,2,2,2,2,2,2,2,2,2,2,2,4),(0.0754220965284081,0.0942775418998476,0.113132987271287,
0.131988590164052,0.150844193056816,0.169699795949581,0.188555398842346,
0.207410844213785,0.226266289585224,0.245121734956664,0.263977180328103,
0.282832783220868,0.301688386113633),.UNSPECIFIED.);
#1307=B_SPLINE_CURVE_WITH_KNOTS('',3,(#8235,#8236,#8237,#8238,#8239,#8240,
#8241,#8242,#8243,#8244,#8245,#8246,#8247,#8248,#8249,#8250,#8251,#8252,
#8253,#8254,#8255,#8256,#8257,#8258,#8259,#8260),.UNSPECIFIED.,.F.,.F.,
(4,2,2,2,2,2,2,2,2,2,2,2,4),(0.,0.0188366744349197,0.0376733488698393,0.0565100213871705,
0.0753466939045017,0.0941833664218329,0.113020038939164,0.131856713374084,
0.150693387809003,0.169530062243923,0.188366736678843,0.207203409196174,
0.226040081713505),.UNSPECIFIED.);
#1308=B_SPLINE_CURVE_WITH_KNOTS('',3,(#8261,#8262,#8263,#8264,#8265,#8266,
#8267,#8268,#8269,#8270),.UNSPECIFIED.,.F.,.F.,(4,2,2,2,4),(0.226040081713505,
0.244876754230836,0.263713426748167,0.282550101183087,0.301386775618007),
 .UNSPECIFIED.);
#1309=B_SPLINE_CURVE_WITH_KNOTS('',3,(#8274,#8275,#8276,#8277,#8278,#8279,
#8280,#8281,#8282,#8283),.UNSPECIFIED.,.F.,.F.,(4,2,2,2,4),(0.,0.0188366744349197,
0.0376733488698393,0.0565100213871705,0.0753466939045016),.UNSPECIFIED.);
#1310=B_SPLINE_CURVE_WITH_KNOTS('',3,(#8285,#8286,#8287,#8288,#8289,#8290,
#8291,#8292,#8293,#8294),.UNSPECIFIED.,.F.,.F.,(4,2,2,2,4),(0.226040081713505,
0.244876754230836,0.263713426748167,0.282550101183087,0.301386775618006),
 .UNSPECIFIED.);
#1311=B_SPLINE_CURVE_WITH_KNOTS('',3,(#8295,#8296,#8297,#8298,#8299,#8300,
#8301,#8302,#8303,#8304,#8305,#8306,#8307,#8308,#8309,#8310,#8311,#8312),
 .UNSPECIFIED.,.F.,.F.,(4,2,2,2,2,2,2,2,4),(0.0753466939045016,0.0941833664218328,
0.113020038939164,0.131856713374084,0.150693387809003,0.169530062243923,
0.188366736678842,0.207203409196173,0.226040081713505),.UNSPECIFIED.);
#1312=B_SPLINE_CURVE_WITH_KNOTS('',3,(#8316,#8317,#8318,#8319,#8320,#8321,
#8322,#8323,#8324,#8325,#8326,#8327,#8328,#8329,#8330,#8331,#8332,#8333),
 .UNSPECIFIED.,.F.,.F.,(4,2,2,2,2,2,2,2,4),(0.0754220965284081,0.0942775418998475,
0.113132987271287,0.131988590164052,0.150844193056816,0.169699795949581,
0.188555398842345,0.207410844213785,0.226266289585224),.UNSPECIFIED.);
#1313=B_SPLINE_CURVE_WITH_KNOTS('',3,(#8335,#8336,#8337,#8338,#8339,#8340,
#8341,#8342,#8343,#8344),.UNSPECIFIED.,.F.,.F.,(4,2,2,2,4),(0.,0.0188556028927646,
0.0377112057855293,0.0565666511569687,0.0754220965284081),.UNSPECIFIED.);
#1314=B_SPLINE_CURVE_WITH_KNOTS('',3,(#8345,#8346,#8347,#8348,#8349,#8350,
#8351,#8352,#8353,#8354),.UNSPECIFIED.,.F.,.F.,(4,2,2,2,4),(0.226266289585224,
0.245121734956664,0.263977180328103,0.282832783220868,0.301688386113632),
 .UNSPECIFIED.);
#1315=B_SPLINE_CURVE_WITH_KNOTS('',3,(#8358,#8359,#8360,#8361,#8362,#8363,
#8364,#8365,#8366,#8367),.UNSPECIFIED.,.F.,.F.,(4,2,2,2,4),(0.,0.0188556028927646,
0.0377112057855293,0.0565666511569687,0.0754220965284081),.UNSPECIFIED.);
#1316=B_SPLINE_CURVE_WITH_KNOTS('',3,(#8368,#8369,#8370,#8371,#8372,#8373,
#8374,#8375,#8376,#8377,#8378,#8379,#8380,#8381,#8382,#8383,#8384,#8385,
#8386,#8387,#8388,#8389,#8390,#8391,#8392,#8393),.UNSPECIFIED.,.F.,.F.,
(4,2,2,2,2,2,2,2,2,2,2,2,4),(0.0754220965284081,0.0942775418998476,0.113132987271287,
0.131988590164052,0.150844193056816,0.169699795949581,0.188555398842345,
0.207410844213785,0.226266289585224,0.245121734956664,0.263977180328103,
0.282832783220868,0.301688386113632),.UNSPECIFIED.);
#1317=B_SPLINE_CURVE_WITH_KNOTS('',3,(#8397,#8398,#8399,#8400,#8401,#8402,
#8403,#8404,#8405,#8406,#8407,#8408,#8409,#8410,#8411,#8412,#8413,#8414,
#8415,#8416,#8417,#8418,#8419,#8420,#8421,#8422),.UNSPECIFIED.,.F.,.F.,
(4,2,2,2,2,2,2,2,2,2,2,2,4),(0.,0.0188366744349194,0.0376733488698389,0.0565100213871702,
0.0753466939045014,0.0941833664218327,0.113020038939164,0.131856713374083,
0.150693387809003,0.169530062243922,0.188366736678842,0.207203409196173,
0.226040081713504),.UNSPECIFIED.);
#1318=B_SPLINE_CURVE_WITH_KNOTS('',3,(#8423,#8424,#8425,#8426,#8427,#8428,
#8429,#8430,#8431,#8432),.UNSPECIFIED.,.F.,.F.,(4,2,2,2,4),(0.226040081713504,
0.244876754230836,0.263713426748167,0.282550101183086,0.301386775618006),
 .UNSPECIFIED.);
#1319=B_SPLINE_CURVE_WITH_KNOTS('',3,(#9675,#9676,#9677,#9678,#9679,#9680,
#9681,#9682,#9683,#9684,#9685,#9686,#9687,#9688,#9689,#9690,#9691,#9692,
#9693,#9694,#9695,#9696,#9697,#9698,#9699,#9700,#9701,#9702,#9703,#9704,
#9705,#9706,#9707,#9708,#9709,#9710,#9711,#9712,#9713,#9714,#9715,#9716,
#9717,#9718,#9719,#9720,#9721,#9722,#9723,#9724,#9725,#9726,#9727,#9728,
#9729,#9730,#9731,#9732,#9733,#9734,#9735,#9736,#9737,#9738,#9739,#9740,
#9741,#9742,#9743,#9744,#9745),.UNSPECIFIED.,.F.,.F.,(4,1,1,1,1,1,1,1,1,
1,1,1,1,1,1,1,1,1,1,1,1,1,1,1,1,1,1,1,1,1,1,1,1,1,1,1,1,1,1,1,1,1,1,1,1,
1,1,1,1,1,1,1,1,1,1,1,1,1,1,1,1,1,1,1,1,1,1,1,4),(0.,0.0178571428571429,
0.0357142857142857,0.0535714285714286,0.0714285714285714,0.0892857142857143,
0.107142857142857,0.125,0.142857142857143,0.150793650793651,0.158730158730159,
0.174603174603175,0.19047619047619,0.202380952380952,0.214285714285714,
0.226190476190476,0.238095238095238,0.25,0.261904761904762,0.267857142857143,
0.273809523809524,0.285714285714286,0.297619047619048,0.30952380952381,
0.321428571428571,0.333333333333333,0.349206349206349,0.365079365079365,
0.380952380952381,0.396825396825397,0.412698412698413,0.428571428571429,
0.446428571428571,0.464285714285714,0.476190476190476,0.488095238095238,
0.5,0.517857142857143,0.535714285714286,0.553571428571429,0.571428571428571,
0.589285714285714,0.607142857142857,0.625,0.642857142857143,0.660714285714286,
0.678571428571428,0.696428571428571,0.714285714285714,0.726190476190476,
0.738095238095238,0.75,0.761904761904762,0.773809523809524,0.785714285714286,
0.797619047619047,0.809523809523809,0.821428571428571,0.833333333333333,
0.845238095238095,0.857142857142857,0.875,0.892857142857143,0.910714285714286,
0.928571428571429,0.946428571428571,0.964285714285714,0.982142857142857,
1.),.UNSPECIFIED.);
#1320=B_SPLINE_CURVE_WITH_KNOTS('',3,(#9784,#9785,#9786,#9787,#9788,#9789,
#9790,#9791,#9792,#9793),.UNSPECIFIED.,.F.,.F.,(4,2,2,2,4),(0.665271585430993,
0.692803751398642,0.755746158887619,0.818688566376595,0.846220732344244),
 .UNSPECIFIED.);
#1321=B_SPLINE_CURVE_WITH_KNOTS('',3,(#9796,#9797,#9798,#9799,#9800,#9801,
#9802,#9803,#9804,#9805),.UNSPECIFIED.,.F.,.F.,(4,2,2,2,4),(0.161440812839248,
0.188972978806896,0.251915386295873,0.314857793784849,0.342389959752498),
 .UNSPECIFIED.);
#1322=B_SPLINE_CURVE_WITH_KNOTS('',3,(#9808,#9809,#9810,#9811,#9812,#9813,
#9814,#9815,#9816,#9817,#9818,#9819,#9820,#9821,#9822,#9823,#9824,#9825,
#9826,#9827,#9828,#9829,#9830,#9831,#9832,#9833,#9834,#9835,#9836,#9837,
#9838,#9839,#9840,#9841),.UNSPECIFIED.,.T.,.F.,(4,2,2,2,2,2,2,2,2,2,2,2,
2,2,2,2,4),(0.,0.0622075173149514,0.124415034629903,0.186622241324509,0.248829448019115,
0.311036654713721,0.373243861408326,0.435451378723278,0.497658896038229,
0.559866413353181,0.622073930668132,0.684281137362738,0.746488344057344,
0.80869555075195,0.870902757446556,0.933110274761507,0.995317792076459),
 .UNSPECIFIED.);
#1323=LINE('',#7014,#1603);
#1324=LINE('',#7056,#1604);
#1325=LINE('',#7063,#1605);
#1326=LINE('',#7070,#1606);
#1327=LINE('',#7077,#1607);
#1328=LINE('',#7084,#1608);
#1329=LINE('',#7091,#1609);
#1330=LINE('',#7097,#1610);
#1331=LINE('',#7106,#1611);
#1332=LINE('',#7112,#1612);
#1333=LINE('',#7128,#1613);
#1334=LINE('',#7130,#1614);
#1335=LINE('',#7136,#1615);
#1336=LINE('',#7143,#1616);
#1337=LINE('',#7150,#1617);
#1338=LINE('',#7157,#1618);
#1339=LINE('',#7164,#1619);
#1340=LINE('',#7176,#1620);
#1341=LINE('',#7181,#1621);
#1342=LINE('',#7194,#1622);
#1343=LINE('',#7198,#1623);
#1344=LINE('',#7200,#1624);
#1345=LINE('',#7271,#1625);
#1346=LINE('',#7312,#1626);
#1347=LINE('',#7318,#1627);
#1348=LINE('',#7360,#1628);
#1349=LINE('',#7365,#1629);
#1350=LINE('',#7370,#1630);
#1351=LINE('',#7384,#1631);
#1352=LINE('',#7388,#1632);
#1353=LINE('',#7390,#1633);
#1354=LINE('',#7400,#1634);
#1355=LINE('',#7444,#1635);
#1356=LINE('',#7451,#1636);
#1357=LINE('',#7462,#1637);
#1358=LINE('',#7465,#1638);
#1359=LINE('',#7471,#1639);
#1360=LINE('',#7481,#1640);
#1361=LINE('',#7485,#1641);
#1362=LINE('',#7492,#1642);
#1363=LINE('',#7498,#1643);
#1364=LINE('',#7503,#1644);
#1365=LINE('',#7505,#1645);
#1366=LINE('',#7552,#1646);
#1367=LINE('',#7624,#1647);
#1368=LINE('',#7696,#1648);
#1369=LINE('',#7768,#1649);
#1370=LINE('',#7840,#1650);
#1371=LINE('',#7912,#1651);
#1372=LINE('',#7990,#1652);
#1373=LINE('',#8071,#1653);
#1374=LINE('',#8152,#1654);
#1375=LINE('',#8233,#1655);
#1376=LINE('',#8314,#1656);
#1377=LINE('',#8395,#1657);
#1378=LINE('',#8436,#1658);
#1379=LINE('',#8437,#1659);
#1380=LINE('',#8438,#1660);
#1381=LINE('',#8440,#1661);
#1382=LINE('',#8447,#1662);
#1383=LINE('',#8453,#1663);
#1384=LINE('',#8454,#1664);
#1385=LINE('',#8455,#1665);
#1386=LINE('',#8457,#1666);
#1387=LINE('',#8469,#1667);
#1388=LINE('',#8475,#1668);
#1389=LINE('',#8481,#1669);
#1390=LINE('',#8488,#1670);
#1391=LINE('',#8490,#1671);
#1392=LINE('',#8492,#1672);
#1393=LINE('',#8493,#1673);
#1394=LINE('',#8496,#1674);
#1395=LINE('',#8498,#1675);
#1396=LINE('',#8499,#1676);
#1397=LINE('',#8502,#1677);
#1398=LINE('',#8504,#1678);
#1399=LINE('',#8505,#1679);
#1400=LINE('',#8508,#1680);
#1401=LINE('',#8510,#1681);
#1402=LINE('',#8511,#1682);
#1403=LINE('',#8513,#1683);
#1404=LINE('',#8514,#1684);
#1405=LINE('',#8522,#1685);
#1406=LINE('',#8528,#1686);
#1407=LINE('',#8534,#1687);
#1408=LINE('',#8540,#1688);
#1409=LINE('',#8546,#1689);
#1410=LINE('',#8552,#1690);
#1411=LINE('',#8557,#1691);
#1412=LINE('',#8559,#1692);
#1413=LINE('',#8561,#1693);
#1414=LINE('',#8562,#1694);
#1415=LINE('',#8566,#1695);
#1416=LINE('',#8568,#1696);
#1417=LINE('',#8570,#1697);
#1418=LINE('',#8571,#1698);
#1419=LINE('',#8574,#1699);
#1420=LINE('',#8576,#1700);
#1421=LINE('',#8577,#1701);
#1422=LINE('',#8580,#1702);
#1423=LINE('',#8582,#1703);
#1424=LINE('',#8583,#1704);
#1425=LINE('',#8585,#1705);
#1426=LINE('',#8586,#1706);
#1427=LINE('',#8591,#1707);
#1428=LINE('',#8595,#1708);
#1429=LINE('',#8597,#1709);
#1430=LINE('',#8598,#1710);
#1431=LINE('',#8601,#1711);
#1432=LINE('',#8603,#1712);
#1433=LINE('',#8604,#1713);
#1434=LINE('',#8606,#1714);
#1435=LINE('',#8607,#1715);
#1436=LINE('',#8614,#1716);
#1437=LINE('',#8616,#1717);
#1438=LINE('',#8618,#1718);
#1439=LINE('',#8620,#1719);
#1440=LINE('',#8622,#1720);
#1441=LINE('',#8623,#1721);
#1442=LINE('',#8629,#1722);
#1443=LINE('',#8631,#1723);
#1444=LINE('',#8633,#1724);
#1445=LINE('',#8635,#1725);
#1446=LINE('',#8637,#1726);
#1447=LINE('',#8638,#1727);
#1448=LINE('',#8642,#1728);
#1449=LINE('',#8643,#1729);
#1450=LINE('',#8645,#1730);
#1451=LINE('',#8647,#1731);
#1452=LINE('',#8649,#1732);
#1453=LINE('',#8651,#1733);
#1454=LINE('',#8655,#1734);
#1455=LINE('',#8663,#1735);
#1456=LINE('',#8667,#1736);
#1457=LINE('',#8671,#1737);
#1458=LINE('',#8676,#1738);
#1459=LINE('',#8682,#1739);
#1460=LINE('',#8688,#1740);
#1461=LINE('',#8701,#1741);
#1462=LINE('',#8713,#1742);
#1463=LINE('',#8716,#1743);
#1464=LINE('',#8719,#1744);
#1465=LINE('',#8725,#1745);
#1466=LINE('',#8734,#1746);
#1467=LINE('',#8740,#1747);
#1468=LINE('',#8749,#1748);
#1469=LINE('',#8755,#1749);
#1470=LINE('',#8761,#1750);
#1471=LINE('',#8767,#1751);
#1472=LINE('',#8773,#1752);
#1473=LINE('',#8779,#1753);
#1474=LINE('',#8785,#1754);
#1475=LINE('',#8791,#1755);
#1476=LINE('',#8800,#1756);
#1477=LINE('',#8806,#1757);
#1478=LINE('',#8816,#1758);
#1479=LINE('',#8820,#1759);
#1480=LINE('',#8832,#1760);
#1481=LINE('',#8835,#1761);
#1482=LINE('',#8839,#1762);
#1483=LINE('',#8843,#1763);
#1484=LINE('',#8854,#1764);
#1485=LINE('',#8857,#1765);
#1486=LINE('',#8865,#1766);
#1487=LINE('',#8868,#1767);
#1488=LINE('',#8876,#1768);
#1489=LINE('',#8879,#1769);
#1490=LINE('',#8883,#1770);
#1491=LINE('',#8887,#1771);
#1492=LINE('',#8895,#1772);
#1493=LINE('',#8907,#1773);
#1494=LINE('',#8913,#1774);
#1495=LINE('',#8919,#1775);
#1496=LINE('',#8925,#1776);
#1497=LINE('',#8931,#1777);
#1498=LINE('',#8937,#1778);
#1499=LINE('',#8943,#1779);
#1500=LINE('',#8949,#1780);
#1501=LINE('',#8957,#1781);
#1502=LINE('',#9754,#1782);
#1503=LINE('',#9761,#1783);
#1504=LINE('',#9770,#1784);
#1505=LINE('',#9778,#1785);
#1506=LINE('',#9807,#1786);
#1507=LINE('',#9843,#1787);
#1508=LINE('',#9848,#1788);
#1509=LINE('',#9854,#1789);
#1510=LINE('',#9865,#1790);
#1511=LINE('',#9869,#1791);
#1512=LINE('',#9873,#1792);
#1513=LINE('',#9880,#1793);
#1514=LINE('',#9884,#1794);
#1515=LINE('',#9888,#1795);
#1516=LINE('',#9893,#1796);
#1517=LINE('',#9895,#1797);
#1518=LINE('',#9897,#1798);
#1519=LINE('',#9898,#1799);
#1520=LINE('',#9901,#1800);
#1521=LINE('',#9903,#1801);
#1522=LINE('',#9904,#1802);
#1523=LINE('',#9907,#1803);
#1524=LINE('',#9909,#1804);
#1525=LINE('',#9910,#1805);
#1526=LINE('',#9913,#1806);
#1527=LINE('',#9915,#1807);
#1528=LINE('',#9916,#1808);
#1529=LINE('',#9919,#1809);
#1530=LINE('',#9921,#1810);
#1531=LINE('',#9922,#1811);
#1532=LINE('',#9924,#1812);
#1533=LINE('',#9925,#1813);
#1534=LINE('',#9933,#1814);
#1535=LINE('',#9939,#1815);
#1536=LINE('',#9955,#1816);
#1537=LINE('',#9976,#1817);
#1538=LINE('',#10001,#1818);
#1539=LINE('',#10002,#1819);
#1540=LINE('',#10004,#1820);
#1541=LINE('',#10006,#1821);
#1542=LINE('',#10011,#1822);
#1543=LINE('',#10014,#1823);
#1544=LINE('',#10016,#1824);
#1545=LINE('',#10024,#1825);
#1546=LINE('',#10026,#1826);
#1547=LINE('',#10028,#1827);
#1548=LINE('',#10029,#1828);
#1549=LINE('',#10032,#1829);
#1550=LINE('',#10034,#1830);
#1551=LINE('',#10035,#1831);
#1552=LINE('',#10038,#1832);
#1553=LINE('',#10040,#1833);
#1554=LINE('',#10041,#1834);
#1555=LINE('',#10044,#1835);
#1556=LINE('',#10046,#1836);
#1557=LINE('',#10047,#1837);
#1558=LINE('',#10050,#1838);
#1559=LINE('',#10052,#1839);
#1560=LINE('',#10053,#1840);
#1561=LINE('',#10055,#1841);
#1562=LINE('',#10056,#1842);
#1563=LINE('',#10064,#1843);
#1564=LINE('',#10068,#1844);
#1565=LINE('',#10072,#1845);
#1566=LINE('',#10084,#1846);
#1567=LINE('',#10089,#1847);
#1568=LINE('',#10091,#1848);
#1569=LINE('',#10093,#1849);
#1570=LINE('',#10094,#1850);
#1571=LINE('',#10097,#1851);
#1572=LINE('',#10099,#1852);
#1573=LINE('',#10100,#1853);
#1574=LINE('',#10103,#1854);
#1575=LINE('',#10105,#1855);
#1576=LINE('',#10106,#1856);
#1577=LINE('',#10108,#1857);
#1578=LINE('',#10109,#1858);
#1579=LINE('',#10119,#1859);
#1580=LINE('',#10123,#1860);
#1581=LINE('',#10127,#1861);
#1582=LINE('',#10134,#1862);
#1583=LINE('',#10138,#1863);
#1584=LINE('',#10142,#1864);
#1585=LINE('',#10147,#1865);
#1586=LINE('',#10149,#1866);
#1587=LINE('',#10151,#1867);
#1588=LINE('',#10152,#1868);
#1589=LINE('',#10155,#1869);
#1590=LINE('',#10157,#1870);
#1591=LINE('',#10158,#1871);
#1592=LINE('',#10161,#1872);
#1593=LINE('',#10163,#1873);
#1594=LINE('',#10164,#1874);
#1595=LINE('',#10167,#1875);
#1596=LINE('',#10169,#1876);
#1597=LINE('',#10170,#1877);
#1598=LINE('',#10173,#1878);
#1599=LINE('',#10175,#1879);
#1600=LINE('',#10176,#1880);
#1601=LINE('',#10178,#1881);
#1602=LINE('',#10179,#1882);
#1603=VECTOR('',#5564,0.165);
#1604=VECTOR('',#5569,0.165);
#1605=VECTOR('',#5578,0.165);
#1606=VECTOR('',#5587,0.165);
#1607=VECTOR('',#5596,0.165);
#1608=VECTOR('',#5605,0.165);
#1609=VECTOR('',#5614,2.24);
#1610=VECTOR('',#5621,2.46);
#1611=VECTOR('',#5632,1.);
#1612=VECTOR('',#5639,1.);
#1613=VECTOR('',#5640,1.);
#1614=VECTOR('',#5641,0.21);
#1615=VECTOR('',#5648,0.21);
#1616=VECTOR('',#5657,0.21);
#1617=VECTOR('',#5666,0.21);
#1618=VECTOR('',#5675,0.21);
#1619=VECTOR('',#5684,0.21);
#1620=VECTOR('',#5699,1.);
#1621=VECTOR('',#5704,1.);
#1622=VECTOR('',#5723,0.2);
#1623=VECTOR('',#5730,0.2);
#1624=VECTOR('',#5731,0.2);
#1625=VECTOR('',#5734,0.685);
#1626=VECTOR('',#5737,0.4);
#1627=VECTOR('',#5744,0.685);
#1628=VECTOR('',#5749,1.);
#1629=VECTOR('',#5754,1.);
#1630=VECTOR('',#5759,1.);
#1631=VECTOR('',#5778,0.4);
#1632=VECTOR('',#5783,1.);
#1633=VECTOR('',#5784,1.);
#1634=VECTOR('',#5799,0.4);
#1635=VECTOR('',#5802,0.685);
#1636=VECTOR('',#5811,0.89);
#1637=VECTOR('',#5826,0.6185);
#1638=VECTOR('',#5829,0.6185);
#1639=VECTOR('',#5836,1.1);
#1640=VECTOR('',#5849,0.6);
#1641=VECTOR('',#5854,0.8);
#1642=VECTOR('',#5863,2.5);
#1643=VECTOR('',#5872,3.31);
#1644=VECTOR('',#5879,4.5);
#1645=VECTOR('',#5880,4.5);
#1646=VECTOR('',#5899,0.05);
#1647=VECTOR('',#5902,0.05);
#1648=VECTOR('',#5905,0.05);
#1649=VECTOR('',#5908,0.05);
#1650=VECTOR('',#5911,0.05);
#1651=VECTOR('',#5914,0.05);
#1652=VECTOR('',#5917,0.0499999999999998);
#1653=VECTOR('',#5920,0.0499999999999998);
#1654=VECTOR('',#5923,0.05);
#1655=VECTOR('',#5926,0.05);
#1656=VECTOR('',#5929,0.05);
#1657=VECTOR('',#5932,0.05);
#1658=VECTOR('',#5937,0.4);
#1659=VECTOR('',#5938,0.4);
#1660=VECTOR('',#5939,0.4);
#1661=VECTOR('',#5940,0.4);
#1662=VECTOR('',#5949,0.6185);
#1663=VECTOR('',#5958,1.2);
#1664=VECTOR('',#5959,1.2);
#1665=VECTOR('',#5960,1.2);
#1666=VECTOR('',#5961,1.2);
#1667=VECTOR('',#5978,2.);
#1668=VECTOR('',#5987,0.685);
#1669=VECTOR('',#5994,1.9);
#1670=VECTOR('',#6003,1.);
#1671=VECTOR('',#6004,1.);
#1672=VECTOR('',#6005,1.);
#1673=VECTOR('',#6006,1.);
#1674=VECTOR('',#6009,1.);
#1675=VECTOR('',#6010,1.);
#1676=VECTOR('',#6011,1.);
#1677=VECTOR('',#6014,1.);
#1678=VECTOR('',#6015,1.);
#1679=VECTOR('',#6016,1.);
#1680=VECTOR('',#6019,1.);
#1681=VECTOR('',#6020,1.);
#1682=VECTOR('',#6021,1.);
#1683=VECTOR('',#6024,1.);
#1684=VECTOR('',#6025,1.);
#1685=VECTOR('',#6036,0.225);
#1686=VECTOR('',#6043,0.225);
#1687=VECTOR('',#6050,0.33);
#1688=VECTOR('',#6057,0.33);
#1689=VECTOR('',#6064,0.33);
#1690=VECTOR('',#6071,0.33);
#1691=VECTOR('',#6076,1.);
#1692=VECTOR('',#6077,1.);
#1693=VECTOR('',#6078,1.);
#1694=VECTOR('',#6079,1.);
#1695=VECTOR('',#6082,1.);
#1696=VECTOR('',#6083,1.);
#1697=VECTOR('',#6084,1.);
#1698=VECTOR('',#6085,1.);
#1699=VECTOR('',#6088,1.);
#1700=VECTOR('',#6089,1.);
#1701=VECTOR('',#6090,1.);
#1702=VECTOR('',#6093,1.);
#1703=VECTOR('',#6094,1.);
#1704=VECTOR('',#6095,1.);
#1705=VECTOR('',#6098,1.);
#1706=VECTOR('',#6099,1.);
#1707=VECTOR('',#6104,3.4);
#1708=VECTOR('',#6109,1.);
#1709=VECTOR('',#6110,1.);
#1710=VECTOR('',#6111,1.);
#1711=VECTOR('',#6114,1.);
#1712=VECTOR('',#6115,1.);
#1713=VECTOR('',#6116,1.);
#1714=VECTOR('',#6119,1.);
#1715=VECTOR('',#6120,1.);
#1716=VECTOR('',#6129,1.);
#1717=VECTOR('',#6130,1.);
#1718=VECTOR('',#6131,1.);
#1719=VECTOR('',#6132,1.);
#1720=VECTOR('',#6133,1.);
#1721=VECTOR('',#6134,1.);
#1722=VECTOR('',#6139,1.);
#1723=VECTOR('',#6140,1.);
#1724=VECTOR('',#6141,1.);
#1725=VECTOR('',#6142,1.);
#1726=VECTOR('',#6143,1.);
#1727=VECTOR('',#6144,1.);
#1728=VECTOR('',#6149,1.);
#1729=VECTOR('',#6150,1.);
#1730=VECTOR('',#6153,1.);
#1731=VECTOR('',#6156,1.);
#1732=VECTOR('',#6159,1.);
#1733=VECTOR('',#6162,1.);
#1734=VECTOR('',#6167,0.685);
#1735=VECTOR('',#6178,0.645);
#1736=VECTOR('',#6183,0.685);
#1737=VECTOR('',#6188,0.645);
#1738=VECTOR('',#6195,0.46);
#1739=VECTOR('',#6202,0.2);
#1740=VECTOR('',#6209,0.6);
#1741=VECTOR('',#6228,0.4);
#1742=VECTOR('',#6243,0.4);
#1743=VECTOR('',#6246,0.15);
#1744=VECTOR('',#6251,0.15);
#1745=VECTOR('',#6258,0.4);
#1746=VECTOR('',#6271,0.16);
#1747=VECTOR('',#6278,2.2);
#1748=VECTOR('',#6291,0.275);
#1749=VECTOR('',#6298,0.275);
#1750=VECTOR('',#6305,0.275);
#1751=VECTOR('',#6312,0.275);
#1752=VECTOR('',#6319,0.275);
#1753=VECTOR('',#6326,0.275);
#1754=VECTOR('',#6333,0.16);
#1755=VECTOR('',#6340,4.);
#1756=VECTOR('',#6353,0.41);
#1757=VECTOR('',#6360,0.6);
#1758=VECTOR('',#6373,0.16);
#1759=VECTOR('',#6378,2.2);
#1760=VECTOR('',#6395,1.);
#1761=VECTOR('',#6398,1.);
#1762=VECTOR('',#6401,1.);
#1763=VECTOR('',#6404,1.);
#1764=VECTOR('',#6419,1.);
#1765=VECTOR('',#6422,1.);
#1766=VECTOR('',#6431,1.);
#1767=VECTOR('',#6434,1.);
#1768=VECTOR('',#6443,1.);
#1769=VECTOR('',#6446,1.);
#1770=VECTOR('',#6449,1.);
#1771=VECTOR('',#6452,1.);
#1772=VECTOR('',#6463,3.);
#1773=VECTOR('',#6482,0.275);
#1774=VECTOR('',#6489,0.275);
#1775=VECTOR('',#6496,0.275);
#1776=VECTOR('',#6503,0.275);
#1777=VECTOR('',#6510,0.275);
#1778=VECTOR('',#6517,0.275);
#1779=VECTOR('',#6524,0.34);
#1780=VECTOR('',#6531,2.5);
#1781=VECTOR('',#6542,4.);
#1782=VECTOR('',#6565,0.6);
#1783=VECTOR('',#6574,1.2);
#1784=VECTOR('',#6587,0.4);
#1785=VECTOR('',#6598,1.);
#1786=VECTOR('',#6607,0.165);
#1787=VECTOR('',#6610,1.);
#1788=VECTOR('',#6615,0.4);
#1789=VECTOR('',#6622,1.5);
#1790=VECTOR('',#6639,0.4);
#1791=VECTOR('',#6644,0.425);
#1792=VECTOR('',#6649,0.41);
#1793=VECTOR('',#6658,0.26);
#1794=VECTOR('',#6663,0.25);
#1795=VECTOR('',#6668,0.225);
#1796=VECTOR('',#6673,1.);
#1797=VECTOR('',#6674,1.);
#1798=VECTOR('',#6675,1.);
#1799=VECTOR('',#6676,1.);
#1800=VECTOR('',#6679,1.);
#1801=VECTOR('',#6680,1.);
#1802=VECTOR('',#6681,1.);
#1803=VECTOR('',#6684,1.);
#1804=VECTOR('',#6685,1.);
#1805=VECTOR('',#6686,1.);
#1806=VECTOR('',#6689,1.);
#1807=VECTOR('',#6690,1.);
#1808=VECTOR('',#6691,1.);
#1809=VECTOR('',#6694,1.);
#1810=VECTOR('',#6695,1.);
#1811=VECTOR('',#6696,1.);
#1812=VECTOR('',#6699,1.);
#1813=VECTOR('',#6700,1.);
#1814=VECTOR('',#6711,0.42);
#1815=VECTOR('',#6718,0.8);
#1816=VECTOR('',#6729,0.734027674973257);
#1817=VECTOR('',#6736,0.734027674973257);
#1818=VECTOR('',#6739,1.);
#1819=VECTOR('',#6740,1.);
#1820=VECTOR('',#6743,1.);
#1821=VECTOR('',#6746,1.);
#1822=VECTOR('',#6751,0.4);
#1823=VECTOR('',#6756,1.);
#1824=VECTOR('',#6759,1.);
#1825=VECTOR('',#6770,1.);
#1826=VECTOR('',#6771,1.);
#1827=VECTOR('',#6772,1.);
#1828=VECTOR('',#6773,1.);
#1829=VECTOR('',#6776,1.);
#1830=VECTOR('',#6777,1.);
#1831=VECTOR('',#6778,1.);
#1832=VECTOR('',#6781,1.);
#1833=VECTOR('',#6782,1.);
#1834=VECTOR('',#6783,1.);
#1835=VECTOR('',#6786,1.);
#1836=VECTOR('',#6787,1.);
#1837=VECTOR('',#6788,1.);
#1838=VECTOR('',#6791,1.);
#1839=VECTOR('',#6792,1.);
#1840=VECTOR('',#6793,1.);
#1841=VECTOR('',#6796,1.);
#1842=VECTOR('',#6797,1.);
#1843=VECTOR('',#6808,0.185);
#1844=VECTOR('',#6813,0.2);
#1845=VECTOR('',#6818,0.1625);
#1846=VECTOR('',#6835,0.225);
#1847=VECTOR('',#6840,1.);
#1848=VECTOR('',#6841,1.);
#1849=VECTOR('',#6842,1.);
#1850=VECTOR('',#6843,1.);
#1851=VECTOR('',#6846,1.);
#1852=VECTOR('',#6847,1.);
#1853=VECTOR('',#6848,1.);
#1854=VECTOR('',#6851,1.);
#1855=VECTOR('',#6852,1.);
#1856=VECTOR('',#6853,1.);
#1857=VECTOR('',#6856,1.);
#1858=VECTOR('',#6857,1.);
#1859=VECTOR('',#6872,0.325);
#1860=VECTOR('',#6877,0.35);
#1861=VECTOR('',#6882,0.335);
#1862=VECTOR('',#6891,0.21);
#1863=VECTOR('',#6896,0.2);
#1864=VECTOR('',#6901,0.18);
#1865=VECTOR('',#6906,1.);
#1866=VECTOR('',#6907,1.);
#1867=VECTOR('',#6908,1.);
#1868=VECTOR('',#6909,1.);
#1869=VECTOR('',#6912,1.);
#1870=VECTOR('',#6913,1.);
#1871=VECTOR('',#6914,1.);
#1872=VECTOR('',#6917,1.);
#1873=VECTOR('',#6918,1.);
#1874=VECTOR('',#6919,1.);
#1875=VECTOR('',#6922,1.);
#1876=VECTOR('',#6923,1.);
#1877=VECTOR('',#6924,1.);
#1878=VECTOR('',#6927,1.);
#1879=VECTOR('',#6928,1.);
#1880=VECTOR('',#6929,1.);
#1881=VECTOR('',#6932,1.);
#1882=VECTOR('',#6933,1.);
#1883=CIRCLE('',#4973,0.165);
#1884=CIRCLE('',#4975,0.165);
#1885=CIRCLE('',#4976,0.165);
#1886=CIRCLE('',#4979,0.165);
#1887=CIRCLE('',#4980,0.165);
#1888=CIRCLE('',#4983,0.165);
#1889=CIRCLE('',#4984,0.165);
#1890=CIRCLE('',#4987,0.165);
#1891=CIRCLE('',#4988,0.165);
#1892=CIRCLE('',#4991,0.165);
#1893=CIRCLE('',#4992,0.165);
#1894=CIRCLE('',#4995,2.24);
#1895=CIRCLE('',#4996,2.24);
#1896=CIRCLE('',#4998,2.46);
#1897=CIRCLE('',#4999,2.46);
#1898=CIRCLE('',#5002,3.31);
#1899=CIRCLE('',#5004,0.21);
#1900=CIRCLE('',#5005,0.21);
#1901=CIRCLE('',#5007,0.21);
#1902=CIRCLE('',#5009,0.21);
#1903=CIRCLE('',#5010,0.21);
#1904=CIRCLE('',#5013,0.21);
#1905=CIRCLE('',#5014,0.21);
#1906=CIRCLE('',#5017,0.21);
#1907=CIRCLE('',#5018,0.21);
#1908=CIRCLE('',#5021,0.21);
#1909=CIRCLE('',#5022,0.21);
#1910=CIRCLE('',#5025,0.21);
#1911=CIRCLE('',#5026,0.21);
#1912=CIRCLE('',#5029,0.685);
#1913=CIRCLE('',#5030,0.685);
#1914=CIRCLE('',#5031,0.2);
#1915=CIRCLE('',#5033,0.2);
#1916=CIRCLE('',#5035,0.2);
#1917=CIRCLE('',#5044,0.2);
#1918=CIRCLE('',#5049,0.4);
#1919=CIRCLE('',#5051,0.685);
#1920=CIRCLE('',#5054,0.4);
#1921=CIRCLE('',#5056,0.4);
#1922=CIRCLE('',#5058,0.4);
#1923=CIRCLE('',#5066,0.4);
#1924=CIRCLE('',#5072,0.4);
#1925=CIRCLE('',#5073,0.4);
#1926=CIRCLE('',#5075,0.4);
#1927=CIRCLE('',#5077,0.685);
#1928=CIRCLE('',#5080,0.89);
#1929=CIRCLE('',#5081,0.89);
#1930=CIRCLE('',#5083,0.6185);
#1931=CIRCLE('',#5085,0.6185);
#1932=CIRCLE('',#5087,0.6185);
#1933=CIRCLE('',#5089,0.6185);
#1934=CIRCLE('',#5091,1.1);
#1935=CIRCLE('',#5092,1.1);
#1936=CIRCLE('',#5094,0.8);
#1937=CIRCLE('',#5097,0.6);
#1938=CIRCLE('',#5098,0.6);
#1939=CIRCLE('',#5100,0.8);
#1940=CIRCLE('',#5103,2.5);
#1941=CIRCLE('',#5104,2.5);
#1942=CIRCLE('',#5107,3.31);
#1943=CIRCLE('',#5110,4.5);
#1944=CIRCLE('',#5111,4.5);
#1945=CIRCLE('',#5116,0.1);
#1946=CIRCLE('',#5117,2.25);
#1947=CIRCLE('',#5132,0.4);
#1948=CIRCLE('',#5133,0.4);
#1949=CIRCLE('',#5136,0.6185);
#1950=CIRCLE('',#5137,0.6185);
#1951=CIRCLE('',#5140,1.2);
#1952=CIRCLE('',#5141,1.2);
#1953=CIRCLE('',#5146,2.);
#1954=CIRCLE('',#5147,0.685);
#1955=CIRCLE('',#5149,2.);
#1956=CIRCLE('',#5152,0.685);
#1957=CIRCLE('',#5155,1.9);
#1958=CIRCLE('',#5156,1.9);
#1959=CIRCLE('',#5168,0.225);
#1960=CIRCLE('',#5169,0.225);
#1961=CIRCLE('',#5171,0.225);
#1962=CIRCLE('',#5172,0.225);
#1963=CIRCLE('',#5174,0.33);
#1964=CIRCLE('',#5175,0.33);
#1965=CIRCLE('',#5177,0.33);
#1966=CIRCLE('',#5178,0.33);
#1967=CIRCLE('',#5180,0.33);
#1968=CIRCLE('',#5181,0.33);
#1969=CIRCLE('',#5183,0.33);
#1970=CIRCLE('',#5184,0.33);
#1971=CIRCLE('',#5191,3.4);
#1972=CIRCLE('',#5192,3.4);
#1973=CIRCLE('',#5200,0.685);
#1974=CIRCLE('',#5202,0.685);
#1975=CIRCLE('',#5210,0.685);
#1976=CIRCLE('',#5212,0.605);
#1977=CIRCLE('',#5213,0.46);
#1978=CIRCLE('',#5216,0.685);
#1979=CIRCLE('',#5218,0.605);
#1980=CIRCLE('',#5220,0.46);
#1981=CIRCLE('',#5224,0.2);
#1982=CIRCLE('',#5225,0.2);
#1983=CIRCLE('',#5227,0.6);
#1984=CIRCLE('',#5228,0.6);
#1985=CIRCLE('',#5233,0.4);
#1986=CIRCLE('',#5234,0.15);
#1987=CIRCLE('',#5236,0.4);
#1988=CIRCLE('',#5238,0.4);
#1989=CIRCLE('',#5239,0.15);
#1990=CIRCLE('',#5241,0.4);
#1991=CIRCLE('',#5242,0.15);
#1992=CIRCLE('',#5245,0.15);
#1993=CIRCLE('',#5249,0.4);
#1994=CIRCLE('',#5250,0.4);
#1995=CIRCLE('',#5255,0.16);
#1996=CIRCLE('',#5256,0.16);
#1997=CIRCLE('',#5258,2.2);
#1998=CIRCLE('',#5259,2.2);
#1999=CIRCLE('',#5264,0.275);
#2000=CIRCLE('',#5265,0.275);
#2001=CIRCLE('',#5267,0.275);
#2002=CIRCLE('',#5268,0.275);
#2003=CIRCLE('',#5270,0.275);
#2004=CIRCLE('',#5271,0.275);
#2005=CIRCLE('',#5273,0.275);
#2006=CIRCLE('',#5274,0.275);
#2007=CIRCLE('',#5276,0.275);
#2008=CIRCLE('',#5277,0.275);
#2009=CIRCLE('',#5279,0.275);
#2010=CIRCLE('',#5280,0.275);
#2011=CIRCLE('',#5282,0.16);
#2012=CIRCLE('',#5283,0.16);
#2013=CIRCLE('',#5285,4.);
#2014=CIRCLE('',#5286,4.);
#2015=CIRCLE('',#5291,0.41);
#2016=CIRCLE('',#5292,0.41);
#2017=CIRCLE('',#5294,0.6);
#2018=CIRCLE('',#5295,0.6);
#2019=CIRCLE('',#5298,2.2);
#2020=CIRCLE('',#5300,0.16);
#2021=CIRCLE('',#5301,0.16);
#2022=CIRCLE('',#5303,2.2);
#2023=CIRCLE('',#5308,3.);
#2024=CIRCLE('',#5309,0.525);
#2025=CIRCLE('',#5311,0.525);
#2026=CIRCLE('',#5313,0.525);
#2027=CIRCLE('',#5314,0.525);
#2028=CIRCLE('',#5316,3.);
#2029=CIRCLE('',#5318,3.);
#2030=CIRCLE('',#5319,0.525);
#2031=CIRCLE('',#5321,0.525);
#2032=CIRCLE('',#5323,3.);
#2033=CIRCLE('',#5324,0.525);
#2034=CIRCLE('',#5326,0.525);
#2035=CIRCLE('',#5328,3.);
#2036=CIRCLE('',#5329,0.525);
#2037=CIRCLE('',#5331,0.525);
#2038=CIRCLE('',#5333,0.525);
#2039=CIRCLE('',#5334,0.525);
#2040=CIRCLE('',#5336,3.);
#2041=CIRCLE('',#5338,3.);
#2042=CIRCLE('',#5339,3.);
#2043=CIRCLE('',#5340,3.);
#2044=CIRCLE('',#5341,3.);
#2045=CIRCLE('',#5342,3.);
#2046=CIRCLE('',#5343,3.);
#2047=CIRCLE('',#5344,3.);
#2048=CIRCLE('',#5345,3.);
#2049=CIRCLE('',#5347,0.275);
#2050=CIRCLE('',#5348,0.275);
#2051=CIRCLE('',#5350,0.275);
#2052=CIRCLE('',#5351,0.275);
#2053=CIRCLE('',#5353,0.275);
#2054=CIRCLE('',#5354,0.275);
#2055=CIRCLE('',#5356,0.275);
#2056=CIRCLE('',#5357,0.275);
#2057=CIRCLE('',#5359,0.275);
#2058=CIRCLE('',#5360,0.275);
#2059=CIRCLE('',#5362,0.275);
#2060=CIRCLE('',#5363,0.275);
#2061=CIRCLE('',#5365,0.34);
#2062=CIRCLE('',#5366,0.34);
#2063=CIRCLE('',#5368,2.5);
#2064=CIRCLE('',#5369,2.5);
#2065=CIRCLE('',#5373,4.);
#2066=CIRCLE('',#5374,4.);
#2067=CIRCLE('',#5378,0.1);
#2068=CIRCLE('',#5379,0.1);
#2069=CIRCLE('',#5384,0.6);
#2070=CIRCLE('',#5385,0.6);
#2071=CIRCLE('',#5388,1.2);
#2072=CIRCLE('',#5389,1.2);
#2073=CIRCLE('',#5394,0.4);
#2074=CIRCLE('',#5395,0.4);
#2075=CIRCLE('',#5400,0.165);
#2076=CIRCLE('',#5401,0.165);
#2077=CIRCLE('',#5403,0.165);
#2078=CIRCLE('',#5406,0.4);
#2079=CIRCLE('',#5407,0.4);
#2080=CIRCLE('',#5409,1.5);
#2081=CIRCLE('',#5410,1.5);
#2082=CIRCLE('',#5415,0.375);
#2083=CIRCLE('',#5417,0.425);
#2084=CIRCLE('',#5419,0.425);
#2085=CIRCLE('',#5421,0.395);
#2086=CIRCLE('',#5423,0.27);
#2087=CIRCLE('',#5425,0.24505);
#2088=CIRCLE('',#5427,0.24505);
#2089=CIRCLE('',#5429,0.2);
#2090=CIRCLE('',#5441,0.42);
#2091=CIRCLE('',#5442,0.42);
#2092=CIRCLE('',#5444,0.8);
#2093=CIRCLE('',#5445,0.8);
#2094=CIRCLE('',#5450,0.6175);
#2095=CIRCLE('',#5452,0.6175);
#2096=CIRCLE('',#5457,0.338975);
#2097=CIRCLE('',#5458,0.338975);
#2098=CIRCLE('',#5473,0.17);
#2099=CIRCLE('',#5475,0.1954);
#2100=CIRCLE('',#5477,0.1954);
#2101=CIRCLE('',#5479,0.125);
#2102=CIRCLE('',#5483,0.131);
#2103=CIRCLE('',#5484,0.6185);
#2104=CIRCLE('',#5487,0.225);
#2105=CIRCLE('',#5488,0.225);
#2106=CIRCLE('',#5497,0.3);
#2107=CIRCLE('',#5499,0.35);
#2108=CIRCLE('',#5501,0.35);
#2109=CIRCLE('',#5503,0.32);
#2110=CIRCLE('',#5505,0.22);
#2111=CIRCLE('',#5507,0.1954);
#2112=CIRCLE('',#5509,0.1954);
#2113=CIRCLE('',#5511,0.16);
#2114=VERTEX_POINT('',#7011);
#2115=VERTEX_POINT('',#7013);
#2116=VERTEX_POINT('',#7015);
#2117=VERTEX_POINT('',#7053);
#2118=VERTEX_POINT('',#7055);
#2119=VERTEX_POINT('',#7060);
#2120=VERTEX_POINT('',#7062);
#2121=VERTEX_POINT('',#7067);
#2122=VERTEX_POINT('',#7069);
#2123=VERTEX_POINT('',#7074);
#2124=VERTEX_POINT('',#7076);
#2125=VERTEX_POINT('',#7081);
#2126=VERTEX_POINT('',#7083);
#2127=VERTEX_POINT('',#7088);
#2128=VERTEX_POINT('',#7090);
#2129=VERTEX_POINT('',#7094);
#2130=VERTEX_POINT('',#7096);
#2131=VERTEX_POINT('',#7101);
#2132=VERTEX_POINT('',#7104);
#2133=VERTEX_POINT('',#7105);
#2134=VERTEX_POINT('',#7107);
#2135=VERTEX_POINT('',#7111);
#2136=VERTEX_POINT('',#7113);
#2137=VERTEX_POINT('',#7129);
#2138=VERTEX_POINT('',#7133);
#2139=VERTEX_POINT('',#7135);
#2140=VERTEX_POINT('',#7140);
#2141=VERTEX_POINT('',#7142);
#2142=VERTEX_POINT('',#7147);
#2143=VERTEX_POINT('',#7149);
#2144=VERTEX_POINT('',#7154);
#2145=VERTEX_POINT('',#7156);
#2146=VERTEX_POINT('',#7161);
#2147=VERTEX_POINT('',#7163);
#2148=VERTEX_POINT('',#7168);
#2149=VERTEX_POINT('',#7171);
#2150=VERTEX_POINT('',#7174);
#2151=VERTEX_POINT('',#7175);
#2152=VERTEX_POINT('',#7179);
#2153=VERTEX_POINT('',#7180);
#2154=VERTEX_POINT('',#7184);
#2155=VERTEX_POINT('',#7188);
#2156=VERTEX_POINT('',#7193);
#2157=VERTEX_POINT('',#7199);
#2158=VERTEX_POINT('',#7236);
#2159=VERTEX_POINT('',#7273);
#2160=VERTEX_POINT('',#7274);
#2161=VERTEX_POINT('',#7311);
#2162=VERTEX_POINT('',#7315);
#2163=VERTEX_POINT('',#7317);
#2164=VERTEX_POINT('',#7319);
#2165=VERTEX_POINT('',#7358);
#2166=VERTEX_POINT('',#7359);
#2167=VERTEX_POINT('',#7363);
#2168=VERTEX_POINT('',#7364);
#2169=VERTEX_POINT('',#7368);
#2170=VERTEX_POINT('',#7369);
#2171=VERTEX_POINT('',#7373);
#2172=VERTEX_POINT('',#7377);
#2173=VERTEX_POINT('',#7381);
#2174=VERTEX_POINT('',#7383);
#2175=VERTEX_POINT('',#7386);
#2176=VERTEX_POINT('',#7389);
#2177=VERTEX_POINT('',#7394);
#2178=VERTEX_POINT('',#7398);
#2179=VERTEX_POINT('',#7402);
#2180=VERTEX_POINT('',#7403);
#2181=VERTEX_POINT('',#7414);
#2182=VERTEX_POINT('',#7443);
#2183=VERTEX_POINT('',#7448);
#2184=VERTEX_POINT('',#7450);
#2185=VERTEX_POINT('',#7454);
#2186=VERTEX_POINT('',#7457);
#2187=VERTEX_POINT('',#7460);
#2188=VERTEX_POINT('',#7464);
#2189=VERTEX_POINT('',#7468);
#2190=VERTEX_POINT('',#7470);
#2191=VERTEX_POINT('',#7474);
#2192=VERTEX_POINT('',#7478);
#2193=VERTEX_POINT('',#7480);
#2194=VERTEX_POINT('',#7484);
#2195=VERTEX_POINT('',#7489);
#2196=VERTEX_POINT('',#7491);
#2197=VERTEX_POINT('',#7496);
#2198=VERTEX_POINT('',#7501);
#2199=VERTEX_POINT('',#7504);
#2200=VERTEX_POINT('',#7511);
#2201=VERTEX_POINT('',#7516);
#2202=VERTEX_POINT('',#7551);
#2203=VERTEX_POINT('',#7588);
#2204=VERTEX_POINT('',#7623);
#2205=VERTEX_POINT('',#7660);
#2206=VERTEX_POINT('',#7695);
#2207=VERTEX_POINT('',#7732);
#2208=VERTEX_POINT('',#7767);
#2209=VERTEX_POINT('',#7804);
#2210=VERTEX_POINT('',#7839);
#2211=VERTEX_POINT('',#7876);
#2212=VERTEX_POINT('',#7911);
#2213=VERTEX_POINT('',#7948);
#2214=VERTEX_POINT('',#7949);
#2215=VERTEX_POINT('',#7960);
#2216=VERTEX_POINT('',#7989);
#2217=VERTEX_POINT('',#7991);
#2218=VERTEX_POINT('',#8010);
#2219=VERTEX_POINT('',#8032);
#2220=VERTEX_POINT('',#8033);
#2221=VERTEX_POINT('',#8070);
#2222=VERTEX_POINT('',#8072);
#2223=VERTEX_POINT('',#8110);
#2224=VERTEX_POINT('',#8111);
#2225=VERTEX_POINT('',#8122);
#2226=VERTEX_POINT('',#8151);
#2227=VERTEX_POINT('',#8153);
#2228=VERTEX_POINT('',#8172);
#2229=VERTEX_POINT('',#8194);
#2230=VERTEX_POINT('',#8195);
#2231=VERTEX_POINT('',#8232);
#2232=VERTEX_POINT('',#8234);
#2233=VERTEX_POINT('',#8272);
#2234=VERTEX_POINT('',#8273);
#2235=VERTEX_POINT('',#8284);
#2236=VERTEX_POINT('',#8313);
#2237=VERTEX_POINT('',#8315);
#2238=VERTEX_POINT('',#8334);
#2239=VERTEX_POINT('',#8356);
#2240=VERTEX_POINT('',#8357);
#2241=VERTEX_POINT('',#8394);
#2242=VERTEX_POINT('',#8396);
#2243=VERTEX_POINT('',#8434);
#2244=VERTEX_POINT('',#8439);
#2245=VERTEX_POINT('',#8444);
#2246=VERTEX_POINT('',#8446);
#2247=VERTEX_POINT('',#8451);
#2248=VERTEX_POINT('',#8456);
#2249=VERTEX_POINT('',#8463);
#2250=VERTEX_POINT('',#8465);
#2251=VERTEX_POINT('',#8468);
#2252=VERTEX_POINT('',#8473);
#2253=VERTEX_POINT('',#8478);
#2254=VERTEX_POINT('',#8480);
#2255=VERTEX_POINT('',#8486);
#2256=VERTEX_POINT('',#8487);
#2257=VERTEX_POINT('',#8489);
#2258=VERTEX_POINT('',#8491);
#2259=VERTEX_POINT('',#8495);
#2260=VERTEX_POINT('',#8497);
#2261=VERTEX_POINT('',#8501);
#2262=VERTEX_POINT('',#8503);
#2263=VERTEX_POINT('',#8507);
#2264=VERTEX_POINT('',#8509);
#2265=VERTEX_POINT('',#8519);
#2266=VERTEX_POINT('',#8521);
#2267=VERTEX_POINT('',#8525);
#2268=VERTEX_POINT('',#8527);
#2269=VERTEX_POINT('',#8531);
#2270=VERTEX_POINT('',#8533);
#2271=VERTEX_POINT('',#8537);
#2272=VERTEX_POINT('',#8539);
#2273=VERTEX_POINT('',#8543);
#2274=VERTEX_POINT('',#8545);
#2275=VERTEX_POINT('',#8549);
#2276=VERTEX_POINT('',#8551);
#2277=VERTEX_POINT('',#8555);
#2278=VERTEX_POINT('',#8556);
#2279=VERTEX_POINT('',#8558);
#2280=VERTEX_POINT('',#8560);
#2281=VERTEX_POINT('',#8564);
#2282=VERTEX_POINT('',#8565);
#2283=VERTEX_POINT('',#8567);
#2284=VERTEX_POINT('',#8569);
#2285=VERTEX_POINT('',#8573);
#2286=VERTEX_POINT('',#8575);
#2287=VERTEX_POINT('',#8579);
#2288=VERTEX_POINT('',#8581);
#2289=VERTEX_POINT('',#8588);
#2290=VERTEX_POINT('',#8590);
#2291=VERTEX_POINT('',#8594);
#2292=VERTEX_POINT('',#8596);
#2293=VERTEX_POINT('',#8600);
#2294=VERTEX_POINT('',#8602);
#2295=VERTEX_POINT('',#8612);
#2296=VERTEX_POINT('',#8613);
#2297=VERTEX_POINT('',#8615);
#2298=VERTEX_POINT('',#8617);
#2299=VERTEX_POINT('',#8619);
#2300=VERTEX_POINT('',#8621);
#2301=VERTEX_POINT('',#8624);
#2302=VERTEX_POINT('',#8627);
#2303=VERTEX_POINT('',#8628);
#2304=VERTEX_POINT('',#8630);
#2305=VERTEX_POINT('',#8632);
#2306=VERTEX_POINT('',#8634);
#2307=VERTEX_POINT('',#8636);
#2308=VERTEX_POINT('',#8639);
#2309=VERTEX_POINT('',#8654);
#2310=VERTEX_POINT('',#8658);
#2311=VERTEX_POINT('',#8660);
#2312=VERTEX_POINT('',#8665);
#2313=VERTEX_POINT('',#8669);
#2314=VERTEX_POINT('',#8673);
#2315=VERTEX_POINT('',#8679);
#2316=VERTEX_POINT('',#8681);
#2317=VERTEX_POINT('',#8685);
#2318=VERTEX_POINT('',#8687);
#2319=VERTEX_POINT('',#8694);
#2320=VERTEX_POINT('',#8696);
#2321=VERTEX_POINT('',#8699);
#2322=VERTEX_POINT('',#8703);
#2323=VERTEX_POINT('',#8705);
#2324=VERTEX_POINT('',#8708);
#2325=VERTEX_POINT('',#8710);
#2326=VERTEX_POINT('',#8715);
#2327=VERTEX_POINT('',#8722);
#2328=VERTEX_POINT('',#8724);
#2329=VERTEX_POINT('',#8731);
#2330=VERTEX_POINT('',#8733);
#2331=VERTEX_POINT('',#8737);
#2332=VERTEX_POINT('',#8739);
#2333=VERTEX_POINT('',#8746);
#2334=VERTEX_POINT('',#8748);
#2335=VERTEX_POINT('',#8752);
#2336=VERTEX_POINT('',#8754);
#2337=VERTEX_POINT('',#8758);
#2338=VERTEX_POINT('',#8760);
#2339=VERTEX_POINT('',#8764);
#2340=VERTEX_POINT('',#8766);
#2341=VERTEX_POINT('',#8770);
#2342=VERTEX_POINT('',#8772);
#2343=VERTEX_POINT('',#8776);
#2344=VERTEX_POINT('',#8778);
#2345=VERTEX_POINT('',#8782);
#2346=VERTEX_POINT('',#8784);
#2347=VERTEX_POINT('',#8788);
#2348=VERTEX_POINT('',#8790);
#2349=VERTEX_POINT('',#8797);
#2350=VERTEX_POINT('',#8799);
#2351=VERTEX_POINT('',#8803);
#2352=VERTEX_POINT('',#8805);
#2353=VERTEX_POINT('',#8810);
#2354=VERTEX_POINT('',#8813);
#2355=VERTEX_POINT('',#8815);
#2356=VERTEX_POINT('',#8819);
#2357=VERTEX_POINT('',#8826);
#2358=VERTEX_POINT('',#8827);
#2359=VERTEX_POINT('',#8831);
#2360=VERTEX_POINT('',#8833);
#2361=VERTEX_POINT('',#8837);
#2362=VERTEX_POINT('',#8838);
#2363=VERTEX_POINT('',#8840);
#2364=VERTEX_POINT('',#8842);
#2365=VERTEX_POINT('',#8848);
#2366=VERTEX_POINT('',#8849);
#2367=VERTEX_POINT('',#8853);
#2368=VERTEX_POINT('',#8855);
#2369=VERTEX_POINT('',#8859);
#2370=VERTEX_POINT('',#8860);
#2371=VERTEX_POINT('',#8864);
#2372=VERTEX_POINT('',#8866);
#2373=VERTEX_POINT('',#8870);
#2374=VERTEX_POINT('',#8871);
#2375=VERTEX_POINT('',#8875);
#2376=VERTEX_POINT('',#8877);
#2377=VERTEX_POINT('',#8881);
#2378=VERTEX_POINT('',#8882);
#2379=VERTEX_POINT('',#8884);
#2380=VERTEX_POINT('',#8886);
#2381=VERTEX_POINT('',#8892);
#2382=VERTEX_POINT('',#8894);
#2383=VERTEX_POINT('',#8904);
#2384=VERTEX_POINT('',#8906);
#2385=VERTEX_POINT('',#8910);
#2386=VERTEX_POINT('',#8912);
#2387=VERTEX_POINT('',#8916);
#2388=VERTEX_POINT('',#8918);
#2389=VERTEX_POINT('',#8922);
#2390=VERTEX_POINT('',#8924);
#2391=VERTEX_POINT('',#8928);
#2392=VERTEX_POINT('',#8930);
#2393=VERTEX_POINT('',#8934);
#2394=VERTEX_POINT('',#8936);
#2395=VERTEX_POINT('',#8940);
#2396=VERTEX_POINT('',#8942);
#2397=VERTEX_POINT('',#8946);
#2398=VERTEX_POINT('',#8948);
#2399=VERTEX_POINT('',#8954);
#2400=VERTEX_POINT('',#8956);
#2401=VERTEX_POINT('',#9672);
#2402=VERTEX_POINT('',#9674);
#2403=VERTEX_POINT('',#9751);
#2404=VERTEX_POINT('',#9753);
#2405=VERTEX_POINT('',#9758);
#2406=VERTEX_POINT('',#9760);
#2407=VERTEX_POINT('',#9767);
#2408=VERTEX_POINT('',#9769);
#2409=VERTEX_POINT('',#9776);
#2410=VERTEX_POINT('',#9777);
#2411=VERTEX_POINT('',#9779);
#2412=VERTEX_POINT('',#9783);
#2413=VERTEX_POINT('',#9794);
#2414=VERTEX_POINT('',#9806);
#2415=VERTEX_POINT('',#9845);
#2416=VERTEX_POINT('',#9847);
#2417=VERTEX_POINT('',#9851);
#2418=VERTEX_POINT('',#9853);
#2419=VERTEX_POINT('',#9860);
#2420=VERTEX_POINT('',#9863);
#2421=VERTEX_POINT('',#9867);
#2422=VERTEX_POINT('',#9871);
#2423=VERTEX_POINT('',#9875);
#2424=VERTEX_POINT('',#9878);
#2425=VERTEX_POINT('',#9882);
#2426=VERTEX_POINT('',#9886);
#2427=VERTEX_POINT('',#9891);
#2428=VERTEX_POINT('',#9892);
#2429=VERTEX_POINT('',#9894);
#2430=VERTEX_POINT('',#9896);
#2431=VERTEX_POINT('',#9900);
#2432=VERTEX_POINT('',#9902);
#2433=VERTEX_POINT('',#9906);
#2434=VERTEX_POINT('',#9908);
#2435=VERTEX_POINT('',#9912);
#2436=VERTEX_POINT('',#9914);
#2437=VERTEX_POINT('',#9918);
#2438=VERTEX_POINT('',#9920);
#2439=VERTEX_POINT('',#9930);
#2440=VERTEX_POINT('',#9932);
#2441=VERTEX_POINT('',#9936);
#2442=VERTEX_POINT('',#9938);
#2443=VERTEX_POINT('',#9945);
#2444=VERTEX_POINT('',#9946);
#2445=VERTEX_POINT('',#9950);
#2446=VERTEX_POINT('',#9954);
#2447=VERTEX_POINT('',#9957);
#2448=VERTEX_POINT('',#9961);
#2449=VERTEX_POINT('',#9965);
#2450=VERTEX_POINT('',#9973);
#2451=VERTEX_POINT('',#9975);
#2452=VERTEX_POINT('',#9977);
#2453=VERTEX_POINT('',#9981);
#2454=VERTEX_POINT('',#9985);
#2455=VERTEX_POINT('',#9989);
#2456=VERTEX_POINT('',#9993);
#2457=VERTEX_POINT('',#10008);
#2458=VERTEX_POINT('',#10010);
#2459=VERTEX_POINT('',#10022);
#2460=VERTEX_POINT('',#10023);
#2461=VERTEX_POINT('',#10025);
#2462=VERTEX_POINT('',#10027);
#2463=VERTEX_POINT('',#10031);
#2464=VERTEX_POINT('',#10033);
#2465=VERTEX_POINT('',#10037);
#2466=VERTEX_POINT('',#10039);
#2467=VERTEX_POINT('',#10043);
#2468=VERTEX_POINT('',#10045);
#2469=VERTEX_POINT('',#10049);
#2470=VERTEX_POINT('',#10051);
#2471=VERTEX_POINT('',#10059);
#2472=VERTEX_POINT('',#10062);
#2473=VERTEX_POINT('',#10066);
#2474=VERTEX_POINT('',#10070);
#2475=VERTEX_POINT('',#10076);
#2476=VERTEX_POINT('',#10081);
#2477=VERTEX_POINT('',#10083);
#2478=VERTEX_POINT('',#10087);
#2479=VERTEX_POINT('',#10088);
#2480=VERTEX_POINT('',#10090);
#2481=VERTEX_POINT('',#10092);
#2482=VERTEX_POINT('',#10096);
#2483=VERTEX_POINT('',#10098);
#2484=VERTEX_POINT('',#10102);
#2485=VERTEX_POINT('',#10104);
#2486=VERTEX_POINT('',#10114);
#2487=VERTEX_POINT('',#10117);
#2488=VERTEX_POINT('',#10121);
#2489=VERTEX_POINT('',#10125);
#2490=VERTEX_POINT('',#10129);
#2491=VERTEX_POINT('',#10132);
#2492=VERTEX_POINT('',#10136);
#2493=VERTEX_POINT('',#10140);
#2494=VERTEX_POINT('',#10145);
#2495=VERTEX_POINT('',#10146);
#2496=VERTEX_POINT('',#10148);
#2497=VERTEX_POINT('',#10150);
#2498=VERTEX_POINT('',#10154);
#2499=VERTEX_POINT('',#10156);
#2500=VERTEX_POINT('',#10160);
#2501=VERTEX_POINT('',#10162);
#2502=VERTEX_POINT('',#10166);
#2503=VERTEX_POINT('',#10168);
#2504=VERTEX_POINT('',#10172);
#2505=VERTEX_POINT('',#10174);
#2506=EDGE_CURVE('',#2114,#2114,#1883,.T.);
#2507=EDGE_CURVE('',#2114,#2115,#1323,.T.);
#2508=EDGE_CURVE('',#2116,#2115,#1265,.T.);
#2509=EDGE_CURVE('',#2115,#2116,#1266,.T.);
#2510=EDGE_CURVE('',#2117,#2117,#1884,.T.);
#2511=EDGE_CURVE('',#2117,#2118,#1324,.T.);
#2512=EDGE_CURVE('',#2118,#2118,#1885,.T.);
#2513=EDGE_CURVE('',#2119,#2119,#1886,.T.);
#2514=EDGE_CURVE('',#2119,#2120,#1325,.T.);
#2515=EDGE_CURVE('',#2120,#2120,#1887,.T.);
#2516=EDGE_CURVE('',#2121,#2121,#1888,.T.);
#2517=EDGE_CURVE('',#2121,#2122,#1326,.T.);
#2518=EDGE_CURVE('',#2122,#2122,#1889,.T.);
#2519=EDGE_CURVE('',#2123,#2123,#1890,.T.);
#2520=EDGE_CURVE('',#2123,#2124,#1327,.T.);
#2521=EDGE_CURVE('',#2124,#2124,#1891,.T.);
#2522=EDGE_CURVE('',#2125,#2125,#1892,.T.);
#2523=EDGE_CURVE('',#2125,#2126,#1328,.T.);
#2524=EDGE_CURVE('',#2126,#2126,#1893,.T.);
#2525=EDGE_CURVE('',#2127,#2127,#1894,.T.);
#2526=EDGE_CURVE('',#2127,#2128,#1329,.T.);
#2527=EDGE_CURVE('',#2128,#2128,#1895,.T.);
#2528=EDGE_CURVE('',#2129,#2129,#1896,.T.);
#2529=EDGE_CURVE('',#2129,#2130,#1330,.T.);
#2530=EDGE_CURVE('',#2130,#2130,#1897,.T.);
#2531=EDGE_CURVE('',#2131,#2131,#1898,.T.);
#2532=EDGE_CURVE('',#2132,#2133,#1331,.T.);
#2533=EDGE_CURVE('',#2132,#2134,#1899,.T.);
#2534=EDGE_CURVE('',#2134,#2133,#1900,.T.);
#2535=EDGE_CURVE('',#2135,#2132,#1332,.T.);
#2536=EDGE_CURVE('',#2136,#2135,#1267,.T.);
#2537=EDGE_CURVE('',#2133,#2136,#1333,.T.);
#2538=EDGE_CURVE('',#2134,#2137,#1334,.T.);
#2539=EDGE_CURVE('',#2137,#2137,#1901,.T.);
#2540=EDGE_CURVE('',#2138,#2138,#1902,.T.);
#2541=EDGE_CURVE('',#2138,#2139,#1335,.T.);
#2542=EDGE_CURVE('',#2139,#2139,#1903,.T.);
#2543=EDGE_CURVE('',#2140,#2140,#1904,.T.);
#2544=EDGE_CURVE('',#2140,#2141,#1336,.T.);
#2545=EDGE_CURVE('',#2141,#2141,#1905,.T.);
#2546=EDGE_CURVE('',#2142,#2142,#1906,.T.);
#2547=EDGE_CURVE('',#2142,#2143,#1337,.T.);
#2548=EDGE_CURVE('',#2143,#2143,#1907,.T.);
#2549=EDGE_CURVE('',#2144,#2144,#1908,.T.);
#2550=EDGE_CURVE('',#2144,#2145,#1338,.T.);
#2551=EDGE_CURVE('',#2145,#2145,#1909,.T.);
#2552=EDGE_CURVE('',#2146,#2146,#1910,.T.);
#2553=EDGE_CURVE('',#2146,#2147,#1339,.T.);
#2554=EDGE_CURVE('',#2147,#2147,#1911,.T.);
#2555=EDGE_CURVE('',#2148,#2136,#1912,.T.);
#2556=EDGE_CURVE('',#2135,#2148,#1913,.T.);
#2557=EDGE_CURVE('',#2149,#2149,#1914,.T.);
#2558=EDGE_CURVE('',#2150,#2151,#1340,.T.);
#2559=EDGE_CURVE('',#2150,#2151,#1915,.T.);
#2560=EDGE_CURVE('',#2152,#2153,#1341,.T.);
#2561=EDGE_CURVE('',#2152,#2153,#1916,.T.);
#2562=EDGE_CURVE('',#2154,#2150,#278,.T.);
#2563=EDGE_CURVE('',#2151,#2154,#279,.T.);
#2564=EDGE_CURVE('',#2155,#2152,#280,.T.);
#2565=EDGE_CURVE('',#2153,#2155,#281,.T.);
#2566=EDGE_CURVE('',#2154,#2155,#282,.T.);
#2567=EDGE_CURVE('',#2154,#2156,#1342,.T.);
#2568=EDGE_CURVE('',#2156,#2156,#1917,.T.);
#2569=EDGE_CURVE('',#2155,#2154,#283,.T.);
#2570=EDGE_CURVE('',#2149,#2154,#1343,.T.);
#2571=EDGE_CURVE('',#2154,#2157,#1344,.T.);
#2572=EDGE_CURVE('',#2157,#2157,#1268,.T.);
#2573=EDGE_CURVE('',#2158,#2158,#1269,.T.);
#2574=EDGE_CURVE('',#2158,#2148,#1345,.T.);
#2575=EDGE_CURVE('',#2159,#2160,#1270,.T.);
#2576=EDGE_CURVE('',#2160,#2159,#1271,.T.);
#2577=EDGE_CURVE('',#2160,#2161,#1346,.T.);
#2578=EDGE_CURVE('',#2161,#2161,#1918,.T.);
#2579=EDGE_CURVE('',#2162,#2162,#1919,.T.);
#2580=EDGE_CURVE('',#2162,#2163,#1347,.T.);
#2581=EDGE_CURVE('',#2164,#2163,#1272,.T.);
#2582=EDGE_CURVE('',#2163,#2164,#1273,.T.);
#2583=EDGE_CURVE('',#2165,#2166,#1348,.T.);
#2584=EDGE_CURVE('',#2166,#2165,#1920,.T.);
#2585=EDGE_CURVE('',#2167,#2168,#1349,.T.);
#2586=EDGE_CURVE('',#2168,#2167,#1921,.T.);
#2587=EDGE_CURVE('',#2169,#2170,#1350,.T.);
#2588=EDGE_CURVE('',#2170,#2169,#1922,.T.);
#2589=EDGE_CURVE('',#2166,#2171,#284,.T.);
#2590=EDGE_CURVE('',#2171,#2165,#285,.T.);
#2591=EDGE_CURVE('',#2168,#2172,#286,.T.);
#2592=EDGE_CURVE('',#2172,#2167,#287,.T.);
#2593=EDGE_CURVE('',#2173,#2173,#1923,.T.);
#2594=EDGE_CURVE('',#2173,#2174,#1351,.T.);
#2595=EDGE_CURVE('',#2171,#2174,#288,.T.);
#2596=EDGE_CURVE('',#2175,#2171,#289,.T.);
#2597=EDGE_CURVE('',#2170,#2175,#1352,.T.);
#2598=EDGE_CURVE('',#2176,#2169,#1353,.T.);
#2599=EDGE_CURVE('',#2172,#2176,#290,.T.);
#2600=EDGE_CURVE('',#2174,#2172,#291,.T.);
#2601=EDGE_CURVE('',#2177,#2175,#1924,.T.);
#2602=EDGE_CURVE('',#2176,#2177,#1925,.T.);
#2603=EDGE_CURVE('',#2178,#2178,#1926,.T.);
#2604=EDGE_CURVE('',#2178,#2177,#1354,.T.);
#2605=EDGE_CURVE('',#2179,#2180,#1274,.T.);
#2606=EDGE_CURVE('',#2181,#2179,#1275,.T.);
#2607=EDGE_CURVE('',#2180,#2181,#1276,.T.);
#2608=EDGE_CURVE('',#2180,#2182,#1355,.T.);
#2609=EDGE_CURVE('',#2182,#2182,#1927,.T.);
#2610=EDGE_CURVE('',#2183,#2183,#1928,.T.);
#2611=EDGE_CURVE('',#2183,#2184,#1356,.T.);
#2612=EDGE_CURVE('',#2184,#2184,#1929,.T.);
#2613=EDGE_CURVE('',#2185,#2185,#1930,.T.);
#2614=EDGE_CURVE('',#2186,#2186,#1931,.T.);
#2615=EDGE_CURVE('',#2187,#2187,#1932,.T.);
#2616=EDGE_CURVE('',#2187,#2186,#1357,.T.);
#2617=EDGE_CURVE('',#2185,#2188,#1358,.T.);
#2618=EDGE_CURVE('',#2188,#2188,#1933,.T.);
#2619=EDGE_CURVE('',#2189,#2189,#1934,.T.);
#2620=EDGE_CURVE('',#2189,#2190,#1359,.T.);
#2621=EDGE_CURVE('',#2190,#2190,#1935,.T.);
#2622=EDGE_CURVE('',#2191,#2191,#1936,.T.);
#2623=EDGE_CURVE('',#2192,#2192,#1937,.T.);
#2624=EDGE_CURVE('',#2192,#2193,#1360,.T.);
#2625=EDGE_CURVE('',#2193,#2193,#1938,.T.);
#2626=EDGE_CURVE('',#2191,#2194,#1361,.T.);
#2627=EDGE_CURVE('',#2194,#2194,#1939,.T.);
#2628=EDGE_CURVE('',#2195,#2195,#1940,.T.);
#2629=EDGE_CURVE('',#2195,#2196,#1362,.T.);
#2630=EDGE_CURVE('',#2196,#2196,#1941,.T.);
#2631=EDGE_CURVE('',#2197,#2197,#1942,.T.);
#2632=EDGE_CURVE('',#2197,#2131,#1363,.T.);
#2633=EDGE_CURVE('',#2198,#2198,#1943,.T.);
#2634=EDGE_CURVE('',#2198,#2180,#1364,.T.);
#2635=EDGE_CURVE('',#2181,#2199,#1365,.T.);
#2636=EDGE_CURVE('',#2199,#2199,#1944,.T.);
#2637=EDGE_CURVE('',#2200,#2200,#1945,.T.);
#2638=EDGE_CURVE('',#2200,#2200,#1946,.T.);
#2639=EDGE_CURVE('',#2201,#2201,#1277,.T.);
#2640=EDGE_CURVE('',#2201,#2202,#1366,.T.);
#2641=EDGE_CURVE('',#2202,#2202,#1278,.T.);
#2642=EDGE_CURVE('',#2203,#2203,#1279,.T.);
#2643=EDGE_CURVE('',#2203,#2204,#1367,.T.);
#2644=EDGE_CURVE('',#2204,#2204,#1280,.T.);
#2645=EDGE_CURVE('',#2205,#2205,#1281,.T.);
#2646=EDGE_CURVE('',#2205,#2206,#1368,.T.);
#2647=EDGE_CURVE('',#2206,#2206,#1282,.T.);
#2648=EDGE_CURVE('',#2207,#2207,#1283,.T.);
#2649=EDGE_CURVE('',#2207,#2208,#1369,.T.);
#2650=EDGE_CURVE('',#2208,#2208,#1284,.T.);
#2651=EDGE_CURVE('',#2209,#2209,#1285,.T.);
#2652=EDGE_CURVE('',#2209,#2210,#1370,.T.);
#2653=EDGE_CURVE('',#2210,#2210,#1286,.T.);
#2654=EDGE_CURVE('',#2211,#2211,#1287,.T.);
#2655=EDGE_CURVE('',#2211,#2212,#1371,.T.);
#2656=EDGE_CURVE('',#2212,#2212,#1288,.T.);
#2657=EDGE_CURVE('',#2213,#2214,#1289,.T.);
#2658=EDGE_CURVE('',#2215,#2213,#1290,.T.);
#2659=EDGE_CURVE('',#2214,#2215,#1291,.T.);
#2660=EDGE_CURVE('',#2214,#2216,#1372,.T.);
#2661=EDGE_CURVE('',#2217,#2216,#1292,.T.);
#2662=EDGE_CURVE('',#2218,#2217,#1293,.T.);
#2663=EDGE_CURVE('',#2216,#2218,#1294,.T.);
#2664=EDGE_CURVE('',#2219,#2220,#1295,.T.);
#2665=EDGE_CURVE('',#2220,#2219,#1296,.T.);
#2666=EDGE_CURVE('',#2220,#2221,#1373,.T.);
#2667=EDGE_CURVE('',#2222,#2221,#1297,.T.);
#2668=EDGE_CURVE('',#2221,#2222,#1298,.T.);
#2669=EDGE_CURVE('',#2223,#2224,#1299,.T.);
#2670=EDGE_CURVE('',#2225,#2223,#1300,.T.);
#2671=EDGE_CURVE('',#2224,#2225,#1301,.T.);
#2672=EDGE_CURVE('',#2224,#2226,#1374,.T.);
#2673=EDGE_CURVE('',#2227,#2226,#1302,.T.);
#2674=EDGE_CURVE('',#2228,#2227,#1303,.T.);
#2675=EDGE_CURVE('',#2226,#2228,#1304,.T.);
#2676=EDGE_CURVE('',#2229,#2230,#1305,.T.);
#2677=EDGE_CURVE('',#2230,#2229,#1306,.T.);
#2678=EDGE_CURVE('',#2230,#2231,#1375,.T.);
#2679=EDGE_CURVE('',#2232,#2231,#1307,.T.);
#2680=EDGE_CURVE('',#2231,#2232,#1308,.T.);
#2681=EDGE_CURVE('',#2233,#2234,#1309,.T.);
#2682=EDGE_CURVE('',#2235,#2233,#1310,.T.);
#2683=EDGE_CURVE('',#2234,#2235,#1311,.T.);
#2684=EDGE_CURVE('',#2234,#2236,#1376,.T.);
#2685=EDGE_CURVE('',#2237,#2236,#1312,.T.);
#2686=EDGE_CURVE('',#2238,#2237,#1313,.T.);
#2687=EDGE_CURVE('',#2236,#2238,#1314,.T.);
#2688=EDGE_CURVE('',#2239,#2240,#1315,.T.);
#2689=EDGE_CURVE('',#2240,#2239,#1316,.T.);
#2690=EDGE_CURVE('',#2240,#2241,#1377,.T.);
#2691=EDGE_CURVE('',#2242,#2241,#1317,.T.);
#2692=EDGE_CURVE('',#2241,#2242,#1318,.T.);
#2693=EDGE_CURVE('',#2243,#2243,#1947,.T.);
#2694=EDGE_CURVE('',#2243,#2217,#1378,.T.);
#2695=EDGE_CURVE('',#2216,#2227,#1379,.T.);
#2696=EDGE_CURVE('',#2226,#2237,#1380,.T.);
#2697=EDGE_CURVE('',#2236,#2244,#1381,.T.);
#2698=EDGE_CURVE('',#2244,#2244,#1948,.T.);
#2699=EDGE_CURVE('',#2245,#2245,#1949,.T.);
#2700=EDGE_CURVE('',#2245,#2246,#1382,.T.);
#2701=EDGE_CURVE('',#2246,#2246,#1950,.T.);
#2702=EDGE_CURVE('',#2247,#2247,#1951,.T.);
#2703=EDGE_CURVE('',#2247,#2234,#1383,.T.);
#2704=EDGE_CURVE('',#2235,#2224,#1384,.T.);
#2705=EDGE_CURVE('',#2225,#2214,#1385,.T.);
#2706=EDGE_CURVE('',#2215,#2248,#1386,.T.);
#2707=EDGE_CURVE('',#2248,#2248,#1952,.T.);
#2708=EDGE_CURVE('',#2249,#2249,#1953,.T.);
#2709=EDGE_CURVE('',#2250,#2250,#1954,.T.);
#2710=EDGE_CURVE('',#2249,#2251,#1387,.T.);
#2711=EDGE_CURVE('',#2251,#2251,#1955,.T.);
#2712=EDGE_CURVE('',#2252,#2252,#1956,.T.);
#2713=EDGE_CURVE('',#2252,#2250,#1388,.T.);
#2714=EDGE_CURVE('',#2253,#2253,#1957,.T.);
#2715=EDGE_CURVE('',#2253,#2254,#1389,.T.);
#2716=EDGE_CURVE('',#2254,#2254,#1958,.T.);
#2717=EDGE_CURVE('',#2255,#2256,#1390,.T.);
#2718=EDGE_CURVE('',#2255,#2257,#1391,.T.);
#2719=EDGE_CURVE('',#2258,#2257,#1392,.T.);
#2720=EDGE_CURVE('',#2256,#2258,#1393,.T.);
#2721=EDGE_CURVE('',#2256,#2259,#1394,.T.);
#2722=EDGE_CURVE('',#2260,#2258,#1395,.T.);
#2723=EDGE_CURVE('',#2259,#2260,#1396,.T.);
#2724=EDGE_CURVE('',#2259,#2261,#1397,.T.);
#2725=EDGE_CURVE('',#2262,#2260,#1398,.T.);
#2726=EDGE_CURVE('',#2261,#2262,#1399,.T.);
#2727=EDGE_CURVE('',#2261,#2263,#1400,.T.);
#2728=EDGE_CURVE('',#2264,#2262,#1401,.T.);
#2729=EDGE_CURVE('',#2263,#2264,#1402,.T.);
#2730=EDGE_CURVE('',#2263,#2255,#1403,.T.);
#2731=EDGE_CURVE('',#2257,#2264,#1404,.T.);
#2732=EDGE_CURVE('',#2265,#2265,#1959,.T.);
#2733=EDGE_CURVE('',#2265,#2266,#1405,.T.);
#2734=EDGE_CURVE('',#2266,#2266,#1960,.T.);
#2735=EDGE_CURVE('',#2267,#2267,#1961,.T.);
#2736=EDGE_CURVE('',#2267,#2268,#1406,.T.);
#2737=EDGE_CURVE('',#2268,#2268,#1962,.T.);
#2738=EDGE_CURVE('',#2269,#2269,#1963,.T.);
#2739=EDGE_CURVE('',#2269,#2270,#1407,.T.);
#2740=EDGE_CURVE('',#2270,#2270,#1964,.T.);
#2741=EDGE_CURVE('',#2271,#2271,#1965,.T.);
#2742=EDGE_CURVE('',#2271,#2272,#1408,.T.);
#2743=EDGE_CURVE('',#2272,#2272,#1966,.T.);
#2744=EDGE_CURVE('',#2273,#2273,#1967,.T.);
#2745=EDGE_CURVE('',#2273,#2274,#1409,.T.);
#2746=EDGE_CURVE('',#2274,#2274,#1968,.T.);
#2747=EDGE_CURVE('',#2275,#2275,#1969,.T.);
#2748=EDGE_CURVE('',#2275,#2276,#1410,.T.);
#2749=EDGE_CURVE('',#2276,#2276,#1970,.T.);
#2750=EDGE_CURVE('',#2277,#2278,#1411,.T.);
#2751=EDGE_CURVE('',#2278,#2279,#1412,.T.);
#2752=EDGE_CURVE('',#2279,#2280,#1413,.T.);
#2753=EDGE_CURVE('',#2280,#2277,#1414,.T.);
#2754=EDGE_CURVE('',#2281,#2282,#1415,.T.);
#2755=EDGE_CURVE('',#2281,#2283,#1416,.T.);
#2756=EDGE_CURVE('',#2283,#2284,#1417,.T.);
#2757=EDGE_CURVE('',#2284,#2282,#1418,.T.);
#2758=EDGE_CURVE('',#2279,#2285,#1419,.T.);
#2759=EDGE_CURVE('',#2286,#2285,#1420,.T.);
#2760=EDGE_CURVE('',#2280,#2286,#1421,.T.);
#2761=EDGE_CURVE('',#2283,#2287,#1422,.T.);
#2762=EDGE_CURVE('',#2288,#2287,#1423,.T.);
#2763=EDGE_CURVE('',#2284,#2288,#1424,.T.);
#2764=EDGE_CURVE('',#2287,#2286,#1425,.T.);
#2765=EDGE_CURVE('',#2285,#2288,#1426,.T.);
#2766=EDGE_CURVE('',#2289,#2289,#1971,.T.);
#2767=EDGE_CURVE('',#2289,#2290,#1427,.T.);
#2768=EDGE_CURVE('',#2290,#2290,#1972,.T.);
#2769=EDGE_CURVE('',#2291,#2277,#1428,.T.);
#2770=EDGE_CURVE('',#2292,#2281,#1429,.T.);
#2771=EDGE_CURVE('',#2291,#2292,#1430,.T.);
#2772=EDGE_CURVE('',#2293,#2291,#1431,.T.);
#2773=EDGE_CURVE('',#2294,#2292,#1432,.T.);
#2774=EDGE_CURVE('',#2293,#2294,#1433,.T.);
#2775=EDGE_CURVE('',#2278,#2293,#1434,.T.);
#2776=EDGE_CURVE('',#2282,#2294,#1435,.T.);
#2777=EDGE_CURVE('',#2295,#2296,#1436,.T.);
#2778=EDGE_CURVE('',#2296,#2297,#1437,.T.);
#2779=EDGE_CURVE('',#2297,#2298,#1438,.T.);
#2780=EDGE_CURVE('',#2298,#2299,#1439,.T.);
#2781=EDGE_CURVE('',#2299,#2300,#1440,.T.);
#2782=EDGE_CURVE('',#2300,#2295,#1441,.T.);
#2783=EDGE_CURVE('',#2301,#2301,#1973,.T.);
#2784=EDGE_CURVE('',#2302,#2303,#1442,.T.);
#2785=EDGE_CURVE('',#2303,#2304,#1443,.T.);
#2786=EDGE_CURVE('',#2304,#2305,#1444,.T.);
#2787=EDGE_CURVE('',#2305,#2306,#1445,.T.);
#2788=EDGE_CURVE('',#2306,#2307,#1446,.T.);
#2789=EDGE_CURVE('',#2307,#2302,#1447,.T.);
#2790=EDGE_CURVE('',#2308,#2308,#1974,.T.);
#2791=EDGE_CURVE('',#2302,#2296,#1448,.T.);
#2792=EDGE_CURVE('',#2297,#2307,#1449,.T.);
#2793=EDGE_CURVE('',#2298,#2306,#1450,.T.);
#2794=EDGE_CURVE('',#2299,#2305,#1451,.T.);
#2795=EDGE_CURVE('',#2300,#2304,#1452,.T.);
#2796=EDGE_CURVE('',#2295,#2303,#1453,.T.);
#2797=EDGE_CURVE('',#2308,#2309,#1454,.T.);
#2798=EDGE_CURVE('',#2309,#2309,#1975,.T.);
#2799=EDGE_CURVE('',#2310,#2310,#1976,.T.);
#2800=EDGE_CURVE('',#2311,#2311,#1977,.T.);
#2801=EDGE_CURVE('',#2309,#2310,#1455,.T.);
#2802=EDGE_CURVE('',#2312,#2312,#1978,.T.);
#2803=EDGE_CURVE('',#2312,#2301,#1456,.T.);
#2804=EDGE_CURVE('',#2313,#2313,#1979,.T.);
#2805=EDGE_CURVE('',#2313,#2312,#1457,.T.);
#2806=EDGE_CURVE('',#2314,#2314,#1980,.T.);
#2807=EDGE_CURVE('',#2314,#2311,#1458,.T.);
#2808=EDGE_CURVE('',#2315,#2315,#1981,.T.);
#2809=EDGE_CURVE('',#2315,#2316,#1459,.T.);
#2810=EDGE_CURVE('',#2316,#2316,#1982,.T.);
#2811=EDGE_CURVE('',#2317,#2317,#1983,.T.);
#2812=EDGE_CURVE('',#2317,#2318,#1460,.T.);
#2813=EDGE_CURVE('',#2318,#2318,#1984,.T.);
#2814=EDGE_CURVE('',#2319,#2319,#1985,.T.);
#2815=EDGE_CURVE('',#2320,#2320,#1986,.T.);
#2816=EDGE_CURVE('',#2321,#2321,#1987,.T.);
#2817=EDGE_CURVE('',#2321,#2319,#1461,.T.);
#2818=EDGE_CURVE('',#2322,#2322,#1988,.T.);
#2819=EDGE_CURVE('',#2323,#2323,#1989,.T.);
#2820=EDGE_CURVE('',#2324,#2324,#1990,.T.);
#2821=EDGE_CURVE('',#2325,#2325,#1991,.T.);
#2822=EDGE_CURVE('',#2322,#2324,#1462,.T.);
#2823=EDGE_CURVE('',#2325,#2326,#1463,.T.);
#2824=EDGE_CURVE('',#2326,#2326,#1992,.T.);
#2825=EDGE_CURVE('',#2320,#2323,#1464,.T.);
#2826=EDGE_CURVE('',#2327,#2327,#1993,.T.);
#2827=EDGE_CURVE('',#2327,#2328,#1465,.T.);
#2828=EDGE_CURVE('',#2328,#2328,#1994,.T.);
#2829=EDGE_CURVE('',#2329,#2329,#1995,.T.);
#2830=EDGE_CURVE('',#2329,#2330,#1466,.T.);
#2831=EDGE_CURVE('',#2330,#2330,#1996,.T.);
#2832=EDGE_CURVE('',#2331,#2331,#1997,.T.);
#2833=EDGE_CURVE('',#2331,#2332,#1467,.T.);
#2834=EDGE_CURVE('',#2332,#2332,#1998,.T.);
#2835=EDGE_CURVE('',#2333,#2333,#1999,.T.);
#2836=EDGE_CURVE('',#2333,#2334,#1468,.T.);
#2837=EDGE_CURVE('',#2334,#2334,#2000,.T.);
#2838=EDGE_CURVE('',#2335,#2335,#2001,.T.);
#2839=EDGE_CURVE('',#2335,#2336,#1469,.T.);
#2840=EDGE_CURVE('',#2336,#2336,#2002,.T.);
#2841=EDGE_CURVE('',#2337,#2337,#2003,.T.);
#2842=EDGE_CURVE('',#2337,#2338,#1470,.T.);
#2843=EDGE_CURVE('',#2338,#2338,#2004,.T.);
#2844=EDGE_CURVE('',#2339,#2339,#2005,.T.);
#2845=EDGE_CURVE('',#2339,#2340,#1471,.T.);
#2846=EDGE_CURVE('',#2340,#2340,#2006,.T.);
#2847=EDGE_CURVE('',#2341,#2341,#2007,.T.);
#2848=EDGE_CURVE('',#2341,#2342,#1472,.T.);
#2849=EDGE_CURVE('',#2342,#2342,#2008,.T.);
#2850=EDGE_CURVE('',#2343,#2343,#2009,.T.);
#2851=EDGE_CURVE('',#2343,#2344,#1473,.T.);
#2852=EDGE_CURVE('',#2344,#2344,#2010,.T.);
#2853=EDGE_CURVE('',#2345,#2345,#2011,.T.);
#2854=EDGE_CURVE('',#2345,#2346,#1474,.T.);
#2855=EDGE_CURVE('',#2346,#2346,#2012,.T.);
#2856=EDGE_CURVE('',#2347,#2347,#2013,.T.);
#2857=EDGE_CURVE('',#2347,#2348,#1475,.T.);
#2858=EDGE_CURVE('',#2348,#2348,#2014,.T.);
#2859=EDGE_CURVE('',#2349,#2349,#2015,.T.);
#2860=EDGE_CURVE('',#2349,#2350,#1476,.T.);
#2861=EDGE_CURVE('',#2350,#2350,#2016,.T.);
#2862=EDGE_CURVE('',#2351,#2351,#2017,.T.);
#2863=EDGE_CURVE('',#2351,#2352,#1477,.T.);
#2864=EDGE_CURVE('',#2352,#2352,#2018,.T.);
#2865=EDGE_CURVE('',#2353,#2353,#2019,.T.);
#2866=EDGE_CURVE('',#2354,#2354,#2020,.T.);
#2867=EDGE_CURVE('',#2354,#2355,#1478,.T.);
#2868=EDGE_CURVE('',#2355,#2355,#2021,.T.);
#2869=EDGE_CURVE('',#2353,#2356,#1479,.T.);
#2870=EDGE_CURVE('',#2356,#2356,#2022,.T.);
#2871=EDGE_CURVE('',#2357,#2358,#2023,.T.);
#2872=EDGE_CURVE('',#2358,#2357,#2024,.T.);
#2873=EDGE_CURVE('',#2359,#2357,#1480,.T.);
#2874=EDGE_CURVE('',#2360,#2359,#2025,.T.);
#2875=EDGE_CURVE('',#2358,#2360,#1481,.T.);
#2876=EDGE_CURVE('',#2361,#2362,#1482,.T.);
#2877=EDGE_CURVE('',#2361,#2363,#2026,.T.);
#2878=EDGE_CURVE('',#2364,#2363,#1483,.T.);
#2879=EDGE_CURVE('',#2362,#2364,#2027,.T.);
#2880=EDGE_CURVE('',#2363,#2361,#2028,.T.);
#2881=EDGE_CURVE('',#2365,#2366,#2029,.T.);
#2882=EDGE_CURVE('',#2366,#2365,#2030,.T.);
#2883=EDGE_CURVE('',#2367,#2365,#1484,.T.);
#2884=EDGE_CURVE('',#2368,#2367,#2031,.T.);
#2885=EDGE_CURVE('',#2366,#2368,#1485,.T.);
#2886=EDGE_CURVE('',#2369,#2370,#2032,.T.);
#2887=EDGE_CURVE('',#2370,#2369,#2033,.T.);
#2888=EDGE_CURVE('',#2371,#2369,#1486,.T.);
#2889=EDGE_CURVE('',#2372,#2371,#2034,.T.);
#2890=EDGE_CURVE('',#2370,#2372,#1487,.T.);
#2891=EDGE_CURVE('',#2373,#2374,#2035,.T.);
#2892=EDGE_CURVE('',#2374,#2373,#2036,.T.);
#2893=EDGE_CURVE('',#2375,#2373,#1488,.T.);
#2894=EDGE_CURVE('',#2376,#2375,#2037,.T.);
#2895=EDGE_CURVE('',#2374,#2376,#1489,.T.);
#2896=EDGE_CURVE('',#2377,#2378,#1490,.T.);
#2897=EDGE_CURVE('',#2377,#2379,#2038,.T.);
#2898=EDGE_CURVE('',#2380,#2379,#1491,.T.);
#2899=EDGE_CURVE('',#2378,#2380,#2039,.T.);
#2900=EDGE_CURVE('',#2379,#2377,#2040,.T.);
#2901=EDGE_CURVE('',#2381,#2381,#2041,.T.);
#2902=EDGE_CURVE('',#2381,#2382,#1492,.T.);
#2903=EDGE_CURVE('',#2375,#2382,#2042,.T.);
#2904=EDGE_CURVE('',#2359,#2376,#2043,.T.);
#2905=EDGE_CURVE('',#2380,#2360,#2044,.T.);
#2906=EDGE_CURVE('',#2364,#2378,#2045,.T.);
#2907=EDGE_CURVE('',#2367,#2362,#2046,.T.);
#2908=EDGE_CURVE('',#2371,#2368,#2047,.T.);
#2909=EDGE_CURVE('',#2382,#2372,#2048,.T.);
#2910=EDGE_CURVE('',#2383,#2383,#2049,.T.);
#2911=EDGE_CURVE('',#2383,#2384,#1493,.T.);
#2912=EDGE_CURVE('',#2384,#2384,#2050,.T.);
#2913=EDGE_CURVE('',#2385,#2385,#2051,.T.);
#2914=EDGE_CURVE('',#2385,#2386,#1494,.T.);
#2915=EDGE_CURVE('',#2386,#2386,#2052,.T.);
#2916=EDGE_CURVE('',#2387,#2387,#2053,.T.);
#2917=EDGE_CURVE('',#2387,#2388,#1495,.T.);
#2918=EDGE_CURVE('',#2388,#2388,#2054,.T.);
#2919=EDGE_CURVE('',#2389,#2389,#2055,.T.);
#2920=EDGE_CURVE('',#2389,#2390,#1496,.T.);
#2921=EDGE_CURVE('',#2390,#2390,#2056,.T.);
#2922=EDGE_CURVE('',#2391,#2391,#2057,.T.);
#2923=EDGE_CURVE('',#2391,#2392,#1497,.T.);
#2924=EDGE_CURVE('',#2392,#2392,#2058,.T.);
#2925=EDGE_CURVE('',#2393,#2393,#2059,.T.);
#2926=EDGE_CURVE('',#2393,#2394,#1498,.T.);
#2927=EDGE_CURVE('',#2394,#2394,#2060,.T.);
#2928=EDGE_CURVE('',#2395,#2395,#2061,.T.);
#2929=EDGE_CURVE('',#2395,#2396,#1499,.T.);
#2930=EDGE_CURVE('',#2396,#2396,#2062,.T.);
#2931=EDGE_CURVE('',#2397,#2397,#2063,.T.);
#2932=EDGE_CURVE('',#2397,#2398,#1500,.T.);
#2933=EDGE_CURVE('',#2398,#2398,#2064,.T.);
#2934=EDGE_CURVE('',#2399,#2399,#2065,.T.);
#2935=EDGE_CURVE('',#2399,#2400,#1501,.T.);
#2936=EDGE_CURVE('',#2400,#2400,#2066,.T.);
#2937=EDGE_CURVE('',#2401,#2401,#2067,.T.);
#2938=EDGE_CURVE('',#2401,#2402,#1319,.T.);
#2939=EDGE_CURVE('',#2402,#2402,#2068,.T.);
#2940=EDGE_CURVE('',#2403,#2403,#2069,.T.);
#2941=EDGE_CURVE('',#2403,#2404,#1502,.T.);
#2942=EDGE_CURVE('',#2404,#2404,#2070,.T.);
#2943=EDGE_CURVE('',#2405,#2405,#2071,.T.);
#2944=EDGE_CURVE('',#2405,#2406,#1503,.T.);
#2945=EDGE_CURVE('',#2406,#2406,#2072,.T.);
#2946=EDGE_CURVE('',#2407,#2407,#2073,.T.);
#2947=EDGE_CURVE('',#2407,#2408,#1504,.T.);
#2948=EDGE_CURVE('',#2408,#2408,#2074,.T.);
#2949=EDGE_CURVE('',#2409,#2410,#1505,.T.);
#2950=EDGE_CURVE('',#2409,#2411,#2075,.T.);
#2951=EDGE_CURVE('',#2411,#2410,#2076,.T.);
#2952=EDGE_CURVE('',#2412,#2409,#1320,.T.);
#2953=EDGE_CURVE('',#2413,#2412,#2077,.T.);
#2954=EDGE_CURVE('',#2410,#2413,#1321,.T.);
#2955=EDGE_CURVE('',#2411,#2414,#1506,.T.);
#2956=EDGE_CURVE('',#2414,#2414,#1322,.T.);
#2957=EDGE_CURVE('',#2413,#2412,#1507,.T.);
#2958=EDGE_CURVE('',#2415,#2415,#2078,.T.);
#2959=EDGE_CURVE('',#2415,#2416,#1508,.T.);
#2960=EDGE_CURVE('',#2416,#2416,#2079,.T.);
#2961=EDGE_CURVE('',#2417,#2417,#2080,.T.);
#2962=EDGE_CURVE('',#2417,#2418,#1509,.T.);
#2963=EDGE_CURVE('',#2418,#2418,#2081,.T.);
#2964=EDGE_CURVE('',#2419,#2419,#2082,.T.);
#2965=EDGE_CURVE('',#2420,#2420,#2083,.T.);
#2966=EDGE_CURVE('',#2420,#2419,#1510,.T.);
#2967=EDGE_CURVE('',#2421,#2421,#2084,.T.);
#2968=EDGE_CURVE('',#2421,#2420,#1511,.T.);
#2969=EDGE_CURVE('',#2422,#2422,#2085,.T.);
#2970=EDGE_CURVE('',#2422,#2421,#1512,.T.);
#2971=EDGE_CURVE('',#2423,#2423,#2086,.T.);
#2972=EDGE_CURVE('',#2424,#2424,#2087,.F.);
#2973=EDGE_CURVE('',#2424,#2423,#1513,.T.);
#2974=EDGE_CURVE('',#2425,#2425,#2088,.F.);
#2975=EDGE_CURVE('',#2425,#2424,#1514,.T.);
#2976=EDGE_CURVE('',#2426,#2426,#2089,.T.);
#2977=EDGE_CURVE('',#2426,#2425,#1515,.T.);
#2978=EDGE_CURVE('',#2427,#2428,#1516,.T.);
#2979=EDGE_CURVE('',#2428,#2429,#1517,.T.);
#2980=EDGE_CURVE('',#2429,#2430,#1518,.T.);
#2981=EDGE_CURVE('',#2427,#2430,#1519,.T.);
#2982=EDGE_CURVE('',#2428,#2431,#1520,.T.);
#2983=EDGE_CURVE('',#2431,#2432,#1521,.T.);
#2984=EDGE_CURVE('',#2432,#2429,#1522,.T.);
#2985=EDGE_CURVE('',#2431,#2433,#1523,.T.);
#2986=EDGE_CURVE('',#2433,#2434,#1524,.T.);
#2987=EDGE_CURVE('',#2434,#2432,#1525,.T.);
#2988=EDGE_CURVE('',#2433,#2435,#1526,.T.);
#2989=EDGE_CURVE('',#2435,#2436,#1527,.T.);
#2990=EDGE_CURVE('',#2436,#2434,#1528,.T.);
#2991=EDGE_CURVE('',#2435,#2437,#1529,.T.);
#2992=EDGE_CURVE('',#2437,#2438,#1530,.T.);
#2993=EDGE_CURVE('',#2438,#2436,#1531,.T.);
#2994=EDGE_CURVE('',#2437,#2427,#1532,.T.);
#2995=EDGE_CURVE('',#2430,#2438,#1533,.T.);
#2996=EDGE_CURVE('',#2439,#2439,#2090,.T.);
#2997=EDGE_CURVE('',#2439,#2440,#1534,.T.);
#2998=EDGE_CURVE('',#2440,#2440,#2091,.T.);
#2999=EDGE_CURVE('',#2441,#2441,#2092,.T.);
#3000=EDGE_CURVE('',#2441,#2442,#1535,.T.);
#3001=EDGE_CURVE('',#2442,#2442,#2093,.T.);
#3002=EDGE_CURVE('',#2443,#2444,#151,.T.);
#3003=EDGE_CURVE('',#2445,#2443,#152,.T.);
#3004=EDGE_CURVE('',#2445,#2446,#1536,.T.);
#3005=EDGE_CURVE('',#2446,#2446,#2094,.T.);
#3006=EDGE_CURVE('',#2447,#2445,#153,.T.);
#3007=EDGE_CURVE('',#2448,#2447,#154,.T.);
#3008=EDGE_CURVE('',#2449,#2448,#155,.T.);
#3009=EDGE_CURVE('',#2444,#2449,#156,.T.);
#3010=EDGE_CURVE('',#2450,#2450,#2095,.T.);
#3011=EDGE_CURVE('',#2450,#2451,#1537,.T.);
#3012=EDGE_CURVE('',#2452,#2451,#157,.T.);
#3013=EDGE_CURVE('',#2453,#2452,#158,.T.);
#3014=EDGE_CURVE('',#2454,#2453,#159,.T.);
#3015=EDGE_CURVE('',#2455,#2454,#160,.T.);
#3016=EDGE_CURVE('',#2456,#2455,#161,.T.);
#3017=EDGE_CURVE('',#2451,#2456,#162,.T.);
#3018=EDGE_CURVE('',#2447,#2456,#1538,.T.);
#3019=EDGE_CURVE('',#2448,#2455,#1539,.T.);
#3020=EDGE_CURVE('',#2445,#2451,#1540,.T.);
#3021=EDGE_CURVE('',#2443,#2452,#1541,.T.);
#3022=EDGE_CURVE('',#2457,#2457,#2096,.F.);
#3023=EDGE_CURVE('',#2457,#2458,#1542,.T.);
#3024=EDGE_CURVE('',#2458,#2458,#2097,.F.);
#3025=EDGE_CURVE('',#2444,#2453,#1543,.T.);
#3026=EDGE_CURVE('',#2449,#2454,#1544,.T.);
#3027=EDGE_CURVE('',#2459,#2460,#1545,.T.);
#3028=EDGE_CURVE('',#2459,#2461,#1546,.T.);
#3029=EDGE_CURVE('',#2461,#2462,#1547,.T.);
#3030=EDGE_CURVE('',#2460,#2462,#1548,.T.);
#3031=EDGE_CURVE('',#2463,#2459,#1549,.T.);
#3032=EDGE_CURVE('',#2463,#2464,#1550,.T.);
#3033=EDGE_CURVE('',#2464,#2461,#1551,.T.);
#3034=EDGE_CURVE('',#2465,#2463,#1552,.T.);
#3035=EDGE_CURVE('',#2465,#2466,#1553,.T.);
#3036=EDGE_CURVE('',#2466,#2464,#1554,.T.);
#3037=EDGE_CURVE('',#2467,#2465,#1555,.T.);
#3038=EDGE_CURVE('',#2467,#2468,#1556,.T.);
#3039=EDGE_CURVE('',#2468,#2466,#1557,.T.);
#3040=EDGE_CURVE('',#2469,#2467,#1558,.T.);
#3041=EDGE_CURVE('',#2469,#2470,#1559,.T.);
#3042=EDGE_CURVE('',#2470,#2468,#1560,.T.);
#3043=EDGE_CURVE('',#2460,#2469,#1561,.T.);
#3044=EDGE_CURVE('',#2462,#2470,#1562,.T.);
#3045=EDGE_CURVE('',#2471,#2471,#2098,.T.);
#3046=EDGE_CURVE('',#2472,#2472,#2099,.T.);
#3047=EDGE_CURVE('',#2472,#2471,#1563,.T.);
#3048=EDGE_CURVE('',#2473,#2473,#2100,.F.);
#3049=EDGE_CURVE('',#2473,#2472,#1564,.T.);
#3050=EDGE_CURVE('',#2474,#2474,#2101,.T.);
#3051=EDGE_CURVE('',#2474,#2473,#1565,.T.);
#3052=EDGE_CURVE('',#2475,#2475,#2102,.T.);
#3053=EDGE_CURVE('',#2475,#2475,#2103,.T.);
#3054=EDGE_CURVE('',#2476,#2476,#2104,.T.);
#3055=EDGE_CURVE('',#2476,#2477,#1566,.T.);
#3056=EDGE_CURVE('',#2477,#2477,#2105,.T.);
#3057=EDGE_CURVE('',#2478,#2479,#1567,.T.);
#3058=EDGE_CURVE('',#2479,#2480,#1568,.T.);
#3059=EDGE_CURVE('',#2481,#2480,#1569,.T.);
#3060=EDGE_CURVE('',#2478,#2481,#1570,.T.);
#3061=EDGE_CURVE('',#2482,#2478,#1571,.T.);
#3062=EDGE_CURVE('',#2483,#2481,#1572,.T.);
#3063=EDGE_CURVE('',#2482,#2483,#1573,.T.);
#3064=EDGE_CURVE('',#2484,#2482,#1574,.T.);
#3065=EDGE_CURVE('',#2485,#2483,#1575,.T.);
#3066=EDGE_CURVE('',#2484,#2485,#1576,.T.);
#3067=EDGE_CURVE('',#2479,#2484,#1577,.T.);
#3068=EDGE_CURVE('',#2480,#2485,#1578,.T.);
#3069=EDGE_CURVE('',#2486,#2486,#2106,.T.);
#3070=EDGE_CURVE('',#2487,#2487,#2107,.T.);
#3071=EDGE_CURVE('',#2487,#2486,#1579,.T.);
#3072=EDGE_CURVE('',#2488,#2488,#2108,.T.);
#3073=EDGE_CURVE('',#2488,#2487,#1580,.T.);
#3074=EDGE_CURVE('',#2489,#2489,#2109,.T.);
#3075=EDGE_CURVE('',#2489,#2488,#1581,.T.);
#3076=EDGE_CURVE('',#2490,#2490,#2110,.T.);
#3077=EDGE_CURVE('',#2491,#2491,#2111,.F.);
#3078=EDGE_CURVE('',#2491,#2490,#1582,.T.);
#3079=EDGE_CURVE('',#2492,#2492,#2112,.F.);
#3080=EDGE_CURVE('',#2492,#2491,#1583,.T.);
#3081=EDGE_CURVE('',#2493,#2493,#2113,.T.);
#3082=EDGE_CURVE('',#2493,#2492,#1584,.T.);
#3083=EDGE_CURVE('',#2494,#2495,#1585,.T.);
#3084=EDGE_CURVE('',#2495,#2496,#1586,.T.);
#3085=EDGE_CURVE('',#2496,#2497,#1587,.T.);
#3086=EDGE_CURVE('',#2494,#2497,#1588,.T.);
#3087=EDGE_CURVE('',#2495,#2498,#1589,.T.);
#3088=EDGE_CURVE('',#2498,#2499,#1590,.T.);
#3089=EDGE_CURVE('',#2499,#2496,#1591,.T.);
#3090=EDGE_CURVE('',#2498,#2500,#1592,.T.);
#3091=EDGE_CURVE('',#2500,#2501,#1593,.T.);
#3092=EDGE_CURVE('',#2501,#2499,#1594,.T.);
#3093=EDGE_CURVE('',#2500,#2502,#1595,.T.);
#3094=EDGE_CURVE('',#2502,#2503,#1596,.T.);
#3095=EDGE_CURVE('',#2503,#2501,#1597,.T.);
#3096=EDGE_CURVE('',#2502,#2504,#1598,.T.);
#3097=EDGE_CURVE('',#2504,#2505,#1599,.T.);
#3098=EDGE_CURVE('',#2505,#2503,#1600,.T.);
#3099=EDGE_CURVE('',#2504,#2494,#1601,.T.);
#3100=EDGE_CURVE('',#2497,#2505,#1602,.T.);
#3101=ORIENTED_EDGE('',*,*,#2506,.F.);
#3102=ORIENTED_EDGE('',*,*,#2507,.T.);
#3103=ORIENTED_EDGE('',*,*,#2508,.F.);
#3104=ORIENTED_EDGE('',*,*,#2509,.F.);
#3105=ORIENTED_EDGE('',*,*,#2507,.F.);
#3106=ORIENTED_EDGE('',*,*,#2510,.F.);
#3107=ORIENTED_EDGE('',*,*,#2511,.T.);
#3108=ORIENTED_EDGE('',*,*,#2512,.T.);
#3109=ORIENTED_EDGE('',*,*,#2511,.F.);
#3110=ORIENTED_EDGE('',*,*,#2512,.F.);
#3111=ORIENTED_EDGE('',*,*,#2513,.F.);
#3112=ORIENTED_EDGE('',*,*,#2514,.T.);
#3113=ORIENTED_EDGE('',*,*,#2515,.T.);
#3114=ORIENTED_EDGE('',*,*,#2514,.F.);
#3115=ORIENTED_EDGE('',*,*,#2515,.F.);
#3116=ORIENTED_EDGE('',*,*,#2516,.F.);
#3117=ORIENTED_EDGE('',*,*,#2517,.T.);
#3118=ORIENTED_EDGE('',*,*,#2518,.T.);
#3119=ORIENTED_EDGE('',*,*,#2517,.F.);
#3120=ORIENTED_EDGE('',*,*,#2518,.F.);
#3121=ORIENTED_EDGE('',*,*,#2519,.F.);
#3122=ORIENTED_EDGE('',*,*,#2520,.T.);
#3123=ORIENTED_EDGE('',*,*,#2521,.T.);
#3124=ORIENTED_EDGE('',*,*,#2520,.F.);
#3125=ORIENTED_EDGE('',*,*,#2521,.F.);
#3126=ORIENTED_EDGE('',*,*,#2522,.F.);
#3127=ORIENTED_EDGE('',*,*,#2523,.T.);
#3128=ORIENTED_EDGE('',*,*,#2524,.T.);
#3129=ORIENTED_EDGE('',*,*,#2523,.F.);
#3130=ORIENTED_EDGE('',*,*,#2524,.F.);
#3131=ORIENTED_EDGE('',*,*,#2525,.F.);
#3132=ORIENTED_EDGE('',*,*,#2526,.T.);
#3133=ORIENTED_EDGE('',*,*,#2527,.T.);
#3134=ORIENTED_EDGE('',*,*,#2526,.F.);
#3135=ORIENTED_EDGE('',*,*,#2528,.F.);
#3136=ORIENTED_EDGE('',*,*,#2529,.T.);
#3137=ORIENTED_EDGE('',*,*,#2530,.T.);
#3138=ORIENTED_EDGE('',*,*,#2529,.F.);
#3139=ORIENTED_EDGE('',*,*,#2530,.F.);
#3140=ORIENTED_EDGE('',*,*,#2527,.F.);
#3141=ORIENTED_EDGE('',*,*,#2531,.F.);
#3142=ORIENTED_EDGE('',*,*,#2528,.T.);
#3143=ORIENTED_EDGE('',*,*,#2522,.T.);
#3144=ORIENTED_EDGE('',*,*,#2519,.T.);
#3145=ORIENTED_EDGE('',*,*,#2516,.T.);
#3146=ORIENTED_EDGE('',*,*,#2513,.T.);
#3147=ORIENTED_EDGE('',*,*,#2532,.F.);
#3148=ORIENTED_EDGE('',*,*,#2533,.T.);
#3149=ORIENTED_EDGE('',*,*,#2534,.T.);
#3150=ORIENTED_EDGE('',*,*,#2535,.F.);
#3151=ORIENTED_EDGE('',*,*,#2536,.F.);
#3152=ORIENTED_EDGE('',*,*,#2537,.F.);
#3153=ORIENTED_EDGE('',*,*,#2534,.F.);
#3154=ORIENTED_EDGE('',*,*,#2538,.T.);
#3155=ORIENTED_EDGE('',*,*,#2539,.F.);
#3156=ORIENTED_EDGE('',*,*,#2538,.F.);
#3157=ORIENTED_EDGE('',*,*,#2533,.F.);
#3158=ORIENTED_EDGE('',*,*,#2540,.F.);
#3159=ORIENTED_EDGE('',*,*,#2541,.T.);
#3160=ORIENTED_EDGE('',*,*,#2542,.F.);
#3161=ORIENTED_EDGE('',*,*,#2541,.F.);
#3162=ORIENTED_EDGE('',*,*,#2540,.T.);
#3163=ORIENTED_EDGE('',*,*,#2543,.F.);
#3164=ORIENTED_EDGE('',*,*,#2544,.T.);
#3165=ORIENTED_EDGE('',*,*,#2545,.F.);
#3166=ORIENTED_EDGE('',*,*,#2544,.F.);
#3167=ORIENTED_EDGE('',*,*,#2543,.T.);
#3168=ORIENTED_EDGE('',*,*,#2546,.F.);
#3169=ORIENTED_EDGE('',*,*,#2547,.T.);
#3170=ORIENTED_EDGE('',*,*,#2548,.F.);
#3171=ORIENTED_EDGE('',*,*,#2547,.F.);
#3172=ORIENTED_EDGE('',*,*,#2546,.T.);
#3173=ORIENTED_EDGE('',*,*,#2549,.F.);
#3174=ORIENTED_EDGE('',*,*,#2550,.T.);
#3175=ORIENTED_EDGE('',*,*,#2551,.F.);
#3176=ORIENTED_EDGE('',*,*,#2550,.F.);
#3177=ORIENTED_EDGE('',*,*,#2549,.T.);
#3178=ORIENTED_EDGE('',*,*,#2552,.F.);
#3179=ORIENTED_EDGE('',*,*,#2553,.T.);
#3180=ORIENTED_EDGE('',*,*,#2554,.F.);
#3181=ORIENTED_EDGE('',*,*,#2553,.F.);
#3182=ORIENTED_EDGE('',*,*,#2552,.T.);
#3183=ORIENTED_EDGE('',*,*,#2535,.T.);
#3184=ORIENTED_EDGE('',*,*,#2532,.T.);
#3185=ORIENTED_EDGE('',*,*,#2537,.T.);
#3186=ORIENTED_EDGE('',*,*,#2555,.F.);
#3187=ORIENTED_EDGE('',*,*,#2556,.F.);
#3188=ORIENTED_EDGE('',*,*,#2557,.T.);
#3189=ORIENTED_EDGE('',*,*,#2558,.F.);
#3190=ORIENTED_EDGE('',*,*,#2559,.T.);
#3191=ORIENTED_EDGE('',*,*,#2560,.F.);
#3192=ORIENTED_EDGE('',*,*,#2561,.T.);
#3193=ORIENTED_EDGE('',*,*,#2562,.F.);
#3194=ORIENTED_EDGE('',*,*,#2563,.F.);
#3195=ORIENTED_EDGE('',*,*,#2559,.F.);
#3196=ORIENTED_EDGE('',*,*,#2564,.F.);
#3197=ORIENTED_EDGE('',*,*,#2565,.F.);
#3198=ORIENTED_EDGE('',*,*,#2561,.F.);
#3199=ORIENTED_EDGE('',*,*,#2566,.F.);
#3200=ORIENTED_EDGE('',*,*,#2567,.T.);
#3201=ORIENTED_EDGE('',*,*,#2568,.F.);
#3202=ORIENTED_EDGE('',*,*,#2567,.F.);
#3203=ORIENTED_EDGE('',*,*,#2569,.F.);
#3204=ORIENTED_EDGE('',*,*,#2557,.F.);
#3205=ORIENTED_EDGE('',*,*,#2570,.T.);
#3206=ORIENTED_EDGE('',*,*,#2566,.T.);
#3207=ORIENTED_EDGE('',*,*,#2564,.T.);
#3208=ORIENTED_EDGE('',*,*,#2560,.T.);
#3209=ORIENTED_EDGE('',*,*,#2565,.T.);
#3210=ORIENTED_EDGE('',*,*,#2569,.T.);
#3211=ORIENTED_EDGE('',*,*,#2571,.T.);
#3212=ORIENTED_EDGE('',*,*,#2572,.F.);
#3213=ORIENTED_EDGE('',*,*,#2571,.F.);
#3214=ORIENTED_EDGE('',*,*,#2562,.T.);
#3215=ORIENTED_EDGE('',*,*,#2558,.T.);
#3216=ORIENTED_EDGE('',*,*,#2563,.T.);
#3217=ORIENTED_EDGE('',*,*,#2570,.F.);
#3218=ORIENTED_EDGE('',*,*,#2573,.F.);
#3219=ORIENTED_EDGE('',*,*,#2574,.T.);
#3220=ORIENTED_EDGE('',*,*,#2555,.T.);
#3221=ORIENTED_EDGE('',*,*,#2536,.T.);
#3222=ORIENTED_EDGE('',*,*,#2556,.T.);
#3223=ORIENTED_EDGE('',*,*,#2574,.F.);
#3224=ORIENTED_EDGE('',*,*,#2575,.F.);
#3225=ORIENTED_EDGE('',*,*,#2576,.F.);
#3226=ORIENTED_EDGE('',*,*,#2577,.T.);
#3227=ORIENTED_EDGE('',*,*,#2578,.F.);
#3228=ORIENTED_EDGE('',*,*,#2577,.F.);
#3229=ORIENTED_EDGE('',*,*,#2579,.F.);
#3230=ORIENTED_EDGE('',*,*,#2580,.T.);
#3231=ORIENTED_EDGE('',*,*,#2581,.F.);
#3232=ORIENTED_EDGE('',*,*,#2582,.F.);
#3233=ORIENTED_EDGE('',*,*,#2580,.F.);
#3234=ORIENTED_EDGE('',*,*,#2579,.T.);
#3235=ORIENTED_EDGE('',*,*,#2578,.T.);
#3236=ORIENTED_EDGE('',*,*,#2583,.F.);
#3237=ORIENTED_EDGE('',*,*,#2584,.F.);
#3238=ORIENTED_EDGE('',*,*,#2585,.F.);
#3239=ORIENTED_EDGE('',*,*,#2586,.F.);
#3240=ORIENTED_EDGE('',*,*,#2587,.F.);
#3241=ORIENTED_EDGE('',*,*,#2588,.F.);
#3242=ORIENTED_EDGE('',*,*,#2589,.F.);
#3243=ORIENTED_EDGE('',*,*,#2584,.T.);
#3244=ORIENTED_EDGE('',*,*,#2590,.F.);
#3245=ORIENTED_EDGE('',*,*,#2591,.F.);
#3246=ORIENTED_EDGE('',*,*,#2586,.T.);
#3247=ORIENTED_EDGE('',*,*,#2592,.F.);
#3248=ORIENTED_EDGE('',*,*,#2593,.F.);
#3249=ORIENTED_EDGE('',*,*,#2594,.T.);
#3250=ORIENTED_EDGE('',*,*,#2595,.F.);
#3251=ORIENTED_EDGE('',*,*,#2596,.F.);
#3252=ORIENTED_EDGE('',*,*,#2597,.F.);
#3253=ORIENTED_EDGE('',*,*,#2588,.T.);
#3254=ORIENTED_EDGE('',*,*,#2598,.F.);
#3255=ORIENTED_EDGE('',*,*,#2599,.F.);
#3256=ORIENTED_EDGE('',*,*,#2600,.F.);
#3257=ORIENTED_EDGE('',*,*,#2594,.F.);
#3258=ORIENTED_EDGE('',*,*,#2598,.T.);
#3259=ORIENTED_EDGE('',*,*,#2587,.T.);
#3260=ORIENTED_EDGE('',*,*,#2597,.T.);
#3261=ORIENTED_EDGE('',*,*,#2601,.F.);
#3262=ORIENTED_EDGE('',*,*,#2602,.F.);
#3263=ORIENTED_EDGE('',*,*,#2603,.F.);
#3264=ORIENTED_EDGE('',*,*,#2604,.T.);
#3265=ORIENTED_EDGE('',*,*,#2601,.T.);
#3266=ORIENTED_EDGE('',*,*,#2596,.T.);
#3267=ORIENTED_EDGE('',*,*,#2590,.T.);
#3268=ORIENTED_EDGE('',*,*,#2583,.T.);
#3269=ORIENTED_EDGE('',*,*,#2589,.T.);
#3270=ORIENTED_EDGE('',*,*,#2595,.T.);
#3271=ORIENTED_EDGE('',*,*,#2600,.T.);
#3272=ORIENTED_EDGE('',*,*,#2592,.T.);
#3273=ORIENTED_EDGE('',*,*,#2585,.T.);
#3274=ORIENTED_EDGE('',*,*,#2591,.T.);
#3275=ORIENTED_EDGE('',*,*,#2599,.T.);
#3276=ORIENTED_EDGE('',*,*,#2602,.T.);
#3277=ORIENTED_EDGE('',*,*,#2604,.F.);
#3278=ORIENTED_EDGE('',*,*,#2605,.F.);
#3279=ORIENTED_EDGE('',*,*,#2606,.F.);
#3280=ORIENTED_EDGE('',*,*,#2607,.F.);
#3281=ORIENTED_EDGE('',*,*,#2608,.T.);
#3282=ORIENTED_EDGE('',*,*,#2609,.T.);
#3283=ORIENTED_EDGE('',*,*,#2608,.F.);
#3284=ORIENTED_EDGE('',*,*,#2508,.T.);
#3285=ORIENTED_EDGE('',*,*,#2509,.T.);
#3286=ORIENTED_EDGE('',*,*,#2609,.F.);
#3287=ORIENTED_EDGE('',*,*,#2603,.T.);
#3288=ORIENTED_EDGE('',*,*,#2610,.F.);
#3289=ORIENTED_EDGE('',*,*,#2611,.T.);
#3290=ORIENTED_EDGE('',*,*,#2612,.T.);
#3291=ORIENTED_EDGE('',*,*,#2611,.F.);
#3292=ORIENTED_EDGE('',*,*,#2612,.F.);
#3293=ORIENTED_EDGE('',*,*,#2613,.F.);
#3294=ORIENTED_EDGE('',*,*,#2610,.T.);
#3295=ORIENTED_EDGE('',*,*,#2614,.F.);
#3296=ORIENTED_EDGE('',*,*,#2615,.F.);
#3297=ORIENTED_EDGE('',*,*,#2616,.T.);
#3298=ORIENTED_EDGE('',*,*,#2614,.T.);
#3299=ORIENTED_EDGE('',*,*,#2616,.F.);
#3300=ORIENTED_EDGE('',*,*,#2613,.T.);
#3301=ORIENTED_EDGE('',*,*,#2617,.T.);
#3302=ORIENTED_EDGE('',*,*,#2618,.F.);
#3303=ORIENTED_EDGE('',*,*,#2617,.F.);
#3304=ORIENTED_EDGE('',*,*,#2619,.F.);
#3305=ORIENTED_EDGE('',*,*,#2620,.T.);
#3306=ORIENTED_EDGE('',*,*,#2621,.T.);
#3307=ORIENTED_EDGE('',*,*,#2620,.F.);
#3308=ORIENTED_EDGE('',*,*,#2622,.F.);
#3309=ORIENTED_EDGE('',*,*,#2618,.T.);
#3310=ORIENTED_EDGE('',*,*,#2621,.F.);
#3311=ORIENTED_EDGE('',*,*,#2615,.T.);
#3312=ORIENTED_EDGE('',*,*,#2623,.F.);
#3313=ORIENTED_EDGE('',*,*,#2624,.T.);
#3314=ORIENTED_EDGE('',*,*,#2625,.F.);
#3315=ORIENTED_EDGE('',*,*,#2624,.F.);
#3316=ORIENTED_EDGE('',*,*,#2572,.T.);
#3317=ORIENTED_EDGE('',*,*,#2622,.T.);
#3318=ORIENTED_EDGE('',*,*,#2626,.T.);
#3319=ORIENTED_EDGE('',*,*,#2627,.T.);
#3320=ORIENTED_EDGE('',*,*,#2626,.F.);
#3321=ORIENTED_EDGE('',*,*,#2627,.F.);
#3322=ORIENTED_EDGE('',*,*,#2623,.T.);
#3323=ORIENTED_EDGE('',*,*,#2628,.F.);
#3324=ORIENTED_EDGE('',*,*,#2629,.T.);
#3325=ORIENTED_EDGE('',*,*,#2630,.F.);
#3326=ORIENTED_EDGE('',*,*,#2629,.F.);
#3327=ORIENTED_EDGE('',*,*,#2575,.T.);
#3328=ORIENTED_EDGE('',*,*,#2576,.T.);
#3329=ORIENTED_EDGE('',*,*,#2628,.T.);
#3330=ORIENTED_EDGE('',*,*,#2568,.T.);
#3331=ORIENTED_EDGE('',*,*,#2625,.T.);
#3332=ORIENTED_EDGE('',*,*,#2631,.F.);
#3333=ORIENTED_EDGE('',*,*,#2632,.T.);
#3334=ORIENTED_EDGE('',*,*,#2531,.T.);
#3335=ORIENTED_EDGE('',*,*,#2632,.F.);
#3336=ORIENTED_EDGE('',*,*,#2525,.T.);
#3337=ORIENTED_EDGE('',*,*,#2593,.T.);
#3338=ORIENTED_EDGE('',*,*,#2619,.T.);
#3339=ORIENTED_EDGE('',*,*,#2633,.F.);
#3340=ORIENTED_EDGE('',*,*,#2634,.T.);
#3341=ORIENTED_EDGE('',*,*,#2607,.T.);
#3342=ORIENTED_EDGE('',*,*,#2635,.T.);
#3343=ORIENTED_EDGE('',*,*,#2636,.T.);
#3344=ORIENTED_EDGE('',*,*,#2635,.F.);
#3345=ORIENTED_EDGE('',*,*,#2606,.T.);
#3346=ORIENTED_EDGE('',*,*,#2605,.T.);
#3347=ORIENTED_EDGE('',*,*,#2634,.F.);
#3348=ORIENTED_EDGE('',*,*,#2573,.T.);
#3349=ORIENTED_EDGE('',*,*,#2581,.T.);
#3350=ORIENTED_EDGE('',*,*,#2582,.T.);
#3351=ORIENTED_EDGE('',*,*,#2633,.T.);
#3352=ORIENTED_EDGE('',*,*,#2630,.T.);
#3353=ORIENTED_EDGE('',*,*,#2554,.T.);
#3354=ORIENTED_EDGE('',*,*,#2551,.T.);
#3355=ORIENTED_EDGE('',*,*,#2548,.T.);
#3356=ORIENTED_EDGE('',*,*,#2545,.T.);
#3357=ORIENTED_EDGE('',*,*,#2542,.T.);
#3358=ORIENTED_EDGE('',*,*,#2539,.T.);
#3359=ORIENTED_EDGE('',*,*,#2636,.F.);
#3360=ORIENTED_EDGE('',*,*,#2506,.T.);
#3361=ORIENTED_EDGE('',*,*,#2510,.T.);
#3362=ORIENTED_EDGE('',*,*,#2631,.T.);
#3363=ORIENTED_EDGE('',*,*,#2637,.F.);
#3364=ORIENTED_EDGE('',*,*,#2638,.T.);
#3365=ORIENTED_EDGE('',*,*,#2637,.T.);
#3366=ORIENTED_EDGE('',*,*,#2638,.F.);
#3367=ORIENTED_EDGE('',*,*,#2639,.F.);
#3368=ORIENTED_EDGE('',*,*,#2640,.T.);
#3369=ORIENTED_EDGE('',*,*,#2641,.F.);
#3370=ORIENTED_EDGE('',*,*,#2640,.F.);
#3371=ORIENTED_EDGE('',*,*,#2642,.F.);
#3372=ORIENTED_EDGE('',*,*,#2643,.T.);
#3373=ORIENTED_EDGE('',*,*,#2644,.F.);
#3374=ORIENTED_EDGE('',*,*,#2643,.F.);
#3375=ORIENTED_EDGE('',*,*,#2645,.F.);
#3376=ORIENTED_EDGE('',*,*,#2646,.T.);
#3377=ORIENTED_EDGE('',*,*,#2647,.F.);
#3378=ORIENTED_EDGE('',*,*,#2646,.F.);
#3379=ORIENTED_EDGE('',*,*,#2648,.F.);
#3380=ORIENTED_EDGE('',*,*,#2649,.T.);
#3381=ORIENTED_EDGE('',*,*,#2650,.F.);
#3382=ORIENTED_EDGE('',*,*,#2649,.F.);
#3383=ORIENTED_EDGE('',*,*,#2651,.F.);
#3384=ORIENTED_EDGE('',*,*,#2652,.T.);
#3385=ORIENTED_EDGE('',*,*,#2653,.F.);
#3386=ORIENTED_EDGE('',*,*,#2652,.F.);
#3387=ORIENTED_EDGE('',*,*,#2654,.F.);
#3388=ORIENTED_EDGE('',*,*,#2655,.T.);
#3389=ORIENTED_EDGE('',*,*,#2656,.F.);
#3390=ORIENTED_EDGE('',*,*,#2655,.F.);
#3391=ORIENTED_EDGE('',*,*,#2657,.F.);
#3392=ORIENTED_EDGE('',*,*,#2658,.F.);
#3393=ORIENTED_EDGE('',*,*,#2659,.F.);
#3394=ORIENTED_EDGE('',*,*,#2660,.T.);
#3395=ORIENTED_EDGE('',*,*,#2661,.F.);
#3396=ORIENTED_EDGE('',*,*,#2662,.F.);
#3397=ORIENTED_EDGE('',*,*,#2663,.F.);
#3398=ORIENTED_EDGE('',*,*,#2660,.F.);
#3399=ORIENTED_EDGE('',*,*,#2664,.F.);
#3400=ORIENTED_EDGE('',*,*,#2665,.F.);
#3401=ORIENTED_EDGE('',*,*,#2666,.T.);
#3402=ORIENTED_EDGE('',*,*,#2667,.F.);
#3403=ORIENTED_EDGE('',*,*,#2668,.F.);
#3404=ORIENTED_EDGE('',*,*,#2666,.F.);
#3405=ORIENTED_EDGE('',*,*,#2669,.F.);
#3406=ORIENTED_EDGE('',*,*,#2670,.F.);
#3407=ORIENTED_EDGE('',*,*,#2671,.F.);
#3408=ORIENTED_EDGE('',*,*,#2672,.T.);
#3409=ORIENTED_EDGE('',*,*,#2673,.F.);
#3410=ORIENTED_EDGE('',*,*,#2674,.F.);
#3411=ORIENTED_EDGE('',*,*,#2675,.F.);
#3412=ORIENTED_EDGE('',*,*,#2672,.F.);
#3413=ORIENTED_EDGE('',*,*,#2676,.F.);
#3414=ORIENTED_EDGE('',*,*,#2677,.F.);
#3415=ORIENTED_EDGE('',*,*,#2678,.T.);
#3416=ORIENTED_EDGE('',*,*,#2679,.F.);
#3417=ORIENTED_EDGE('',*,*,#2680,.F.);
#3418=ORIENTED_EDGE('',*,*,#2678,.F.);
#3419=ORIENTED_EDGE('',*,*,#2681,.F.);
#3420=ORIENTED_EDGE('',*,*,#2682,.F.);
#3421=ORIENTED_EDGE('',*,*,#2683,.F.);
#3422=ORIENTED_EDGE('',*,*,#2684,.T.);
#3423=ORIENTED_EDGE('',*,*,#2685,.F.);
#3424=ORIENTED_EDGE('',*,*,#2686,.F.);
#3425=ORIENTED_EDGE('',*,*,#2687,.F.);
#3426=ORIENTED_EDGE('',*,*,#2684,.F.);
#3427=ORIENTED_EDGE('',*,*,#2688,.F.);
#3428=ORIENTED_EDGE('',*,*,#2689,.F.);
#3429=ORIENTED_EDGE('',*,*,#2690,.T.);
#3430=ORIENTED_EDGE('',*,*,#2691,.F.);
#3431=ORIENTED_EDGE('',*,*,#2692,.F.);
#3432=ORIENTED_EDGE('',*,*,#2690,.F.);
#3433=ORIENTED_EDGE('',*,*,#2693,.F.);
#3434=ORIENTED_EDGE('',*,*,#2694,.T.);
#3435=ORIENTED_EDGE('',*,*,#2661,.T.);
#3436=ORIENTED_EDGE('',*,*,#2695,.T.);
#3437=ORIENTED_EDGE('',*,*,#2673,.T.);
#3438=ORIENTED_EDGE('',*,*,#2696,.T.);
#3439=ORIENTED_EDGE('',*,*,#2685,.T.);
#3440=ORIENTED_EDGE('',*,*,#2697,.T.);
#3441=ORIENTED_EDGE('',*,*,#2698,.F.);
#3442=ORIENTED_EDGE('',*,*,#2697,.F.);
#3443=ORIENTED_EDGE('',*,*,#2687,.T.);
#3444=ORIENTED_EDGE('',*,*,#2686,.T.);
#3445=ORIENTED_EDGE('',*,*,#2696,.F.);
#3446=ORIENTED_EDGE('',*,*,#2675,.T.);
#3447=ORIENTED_EDGE('',*,*,#2674,.T.);
#3448=ORIENTED_EDGE('',*,*,#2695,.F.);
#3449=ORIENTED_EDGE('',*,*,#2663,.T.);
#3450=ORIENTED_EDGE('',*,*,#2662,.T.);
#3451=ORIENTED_EDGE('',*,*,#2694,.F.);
#3452=ORIENTED_EDGE('',*,*,#2642,.T.);
#3453=ORIENTED_EDGE('',*,*,#2641,.T.);
#3454=ORIENTED_EDGE('',*,*,#2648,.T.);
#3455=ORIENTED_EDGE('',*,*,#2647,.T.);
#3456=ORIENTED_EDGE('',*,*,#2654,.T.);
#3457=ORIENTED_EDGE('',*,*,#2653,.T.);
#3458=ORIENTED_EDGE('',*,*,#2664,.T.);
#3459=ORIENTED_EDGE('',*,*,#2665,.T.);
#3460=ORIENTED_EDGE('',*,*,#2676,.T.);
#3461=ORIENTED_EDGE('',*,*,#2677,.T.);
#3462=ORIENTED_EDGE('',*,*,#2688,.T.);
#3463=ORIENTED_EDGE('',*,*,#2689,.T.);
#3464=ORIENTED_EDGE('',*,*,#2693,.T.);
#3465=ORIENTED_EDGE('',*,*,#2699,.F.);
#3466=ORIENTED_EDGE('',*,*,#2700,.T.);
#3467=ORIENTED_EDGE('',*,*,#2701,.F.);
#3468=ORIENTED_EDGE('',*,*,#2700,.F.);
#3469=ORIENTED_EDGE('',*,*,#2699,.T.);
#3470=ORIENTED_EDGE('',*,*,#2698,.T.);
#3471=ORIENTED_EDGE('',*,*,#2702,.F.);
#3472=ORIENTED_EDGE('',*,*,#2703,.T.);
#3473=ORIENTED_EDGE('',*,*,#2683,.T.);
#3474=ORIENTED_EDGE('',*,*,#2704,.T.);
#3475=ORIENTED_EDGE('',*,*,#2671,.T.);
#3476=ORIENTED_EDGE('',*,*,#2705,.T.);
#3477=ORIENTED_EDGE('',*,*,#2659,.T.);
#3478=ORIENTED_EDGE('',*,*,#2706,.T.);
#3479=ORIENTED_EDGE('',*,*,#2707,.T.);
#3480=ORIENTED_EDGE('',*,*,#2706,.F.);
#3481=ORIENTED_EDGE('',*,*,#2658,.T.);
#3482=ORIENTED_EDGE('',*,*,#2657,.T.);
#3483=ORIENTED_EDGE('',*,*,#2705,.F.);
#3484=ORIENTED_EDGE('',*,*,#2670,.T.);
#3485=ORIENTED_EDGE('',*,*,#2669,.T.);
#3486=ORIENTED_EDGE('',*,*,#2704,.F.);
#3487=ORIENTED_EDGE('',*,*,#2682,.T.);
#3488=ORIENTED_EDGE('',*,*,#2681,.T.);
#3489=ORIENTED_EDGE('',*,*,#2703,.F.);
#3490=ORIENTED_EDGE('',*,*,#2644,.T.);
#3491=ORIENTED_EDGE('',*,*,#2639,.T.);
#3492=ORIENTED_EDGE('',*,*,#2650,.T.);
#3493=ORIENTED_EDGE('',*,*,#2645,.T.);
#3494=ORIENTED_EDGE('',*,*,#2656,.T.);
#3495=ORIENTED_EDGE('',*,*,#2651,.T.);
#3496=ORIENTED_EDGE('',*,*,#2667,.T.);
#3497=ORIENTED_EDGE('',*,*,#2668,.T.);
#3498=ORIENTED_EDGE('',*,*,#2679,.T.);
#3499=ORIENTED_EDGE('',*,*,#2680,.T.);
#3500=ORIENTED_EDGE('',*,*,#2691,.T.);
#3501=ORIENTED_EDGE('',*,*,#2692,.T.);
#3502=ORIENTED_EDGE('',*,*,#2702,.T.);
#3503=ORIENTED_EDGE('',*,*,#2701,.T.);
#3504=ORIENTED_EDGE('',*,*,#2707,.F.);
#3505=ORIENTED_EDGE('',*,*,#2708,.T.);
#3506=ORIENTED_EDGE('',*,*,#2709,.F.);
#3507=ORIENTED_EDGE('',*,*,#2708,.F.);
#3508=ORIENTED_EDGE('',*,*,#2710,.T.);
#3509=ORIENTED_EDGE('',*,*,#2711,.T.);
#3510=ORIENTED_EDGE('',*,*,#2710,.F.);
#3511=ORIENTED_EDGE('',*,*,#2711,.F.);
#3512=ORIENTED_EDGE('',*,*,#2712,.F.);
#3513=ORIENTED_EDGE('',*,*,#2713,.T.);
#3514=ORIENTED_EDGE('',*,*,#2709,.T.);
#3515=ORIENTED_EDGE('',*,*,#2713,.F.);
#3516=ORIENTED_EDGE('',*,*,#2712,.T.);
#3517=ORIENTED_EDGE('',*,*,#2714,.F.);
#3518=ORIENTED_EDGE('',*,*,#2715,.T.);
#3519=ORIENTED_EDGE('',*,*,#2716,.T.);
#3520=ORIENTED_EDGE('',*,*,#2715,.F.);
#3521=ORIENTED_EDGE('',*,*,#2714,.T.);
#3522=ORIENTED_EDGE('',*,*,#2716,.F.);
#3523=ORIENTED_EDGE('',*,*,#2717,.F.);
#3524=ORIENTED_EDGE('',*,*,#2718,.T.);
#3525=ORIENTED_EDGE('',*,*,#2719,.F.);
#3526=ORIENTED_EDGE('',*,*,#2720,.F.);
#3527=ORIENTED_EDGE('',*,*,#2721,.F.);
#3528=ORIENTED_EDGE('',*,*,#2720,.T.);
#3529=ORIENTED_EDGE('',*,*,#2722,.F.);
#3530=ORIENTED_EDGE('',*,*,#2723,.F.);
#3531=ORIENTED_EDGE('',*,*,#2724,.F.);
#3532=ORIENTED_EDGE('',*,*,#2723,.T.);
#3533=ORIENTED_EDGE('',*,*,#2725,.F.);
#3534=ORIENTED_EDGE('',*,*,#2726,.F.);
#3535=ORIENTED_EDGE('',*,*,#2727,.F.);
#3536=ORIENTED_EDGE('',*,*,#2726,.T.);
#3537=ORIENTED_EDGE('',*,*,#2728,.F.);
#3538=ORIENTED_EDGE('',*,*,#2729,.F.);
#3539=ORIENTED_EDGE('',*,*,#2730,.F.);
#3540=ORIENTED_EDGE('',*,*,#2729,.T.);
#3541=ORIENTED_EDGE('',*,*,#2731,.F.);
#3542=ORIENTED_EDGE('',*,*,#2718,.F.);
#3543=ORIENTED_EDGE('',*,*,#2731,.T.);
#3544=ORIENTED_EDGE('',*,*,#2728,.T.);
#3545=ORIENTED_EDGE('',*,*,#2725,.T.);
#3546=ORIENTED_EDGE('',*,*,#2722,.T.);
#3547=ORIENTED_EDGE('',*,*,#2719,.T.);
#3548=ORIENTED_EDGE('',*,*,#2730,.T.);
#3549=ORIENTED_EDGE('',*,*,#2717,.T.);
#3550=ORIENTED_EDGE('',*,*,#2721,.T.);
#3551=ORIENTED_EDGE('',*,*,#2724,.T.);
#3552=ORIENTED_EDGE('',*,*,#2727,.T.);
#3553=ORIENTED_EDGE('',*,*,#2732,.F.);
#3554=ORIENTED_EDGE('',*,*,#2733,.T.);
#3555=ORIENTED_EDGE('',*,*,#2734,.F.);
#3556=ORIENTED_EDGE('',*,*,#2733,.F.);
#3557=ORIENTED_EDGE('',*,*,#2735,.F.);
#3558=ORIENTED_EDGE('',*,*,#2736,.T.);
#3559=ORIENTED_EDGE('',*,*,#2737,.F.);
#3560=ORIENTED_EDGE('',*,*,#2736,.F.);
#3561=ORIENTED_EDGE('',*,*,#2738,.F.);
#3562=ORIENTED_EDGE('',*,*,#2739,.T.);
#3563=ORIENTED_EDGE('',*,*,#2740,.F.);
#3564=ORIENTED_EDGE('',*,*,#2739,.F.);
#3565=ORIENTED_EDGE('',*,*,#2741,.F.);
#3566=ORIENTED_EDGE('',*,*,#2742,.T.);
#3567=ORIENTED_EDGE('',*,*,#2743,.F.);
#3568=ORIENTED_EDGE('',*,*,#2742,.F.);
#3569=ORIENTED_EDGE('',*,*,#2744,.F.);
#3570=ORIENTED_EDGE('',*,*,#2745,.T.);
#3571=ORIENTED_EDGE('',*,*,#2746,.F.);
#3572=ORIENTED_EDGE('',*,*,#2745,.F.);
#3573=ORIENTED_EDGE('',*,*,#2747,.F.);
#3574=ORIENTED_EDGE('',*,*,#2748,.T.);
#3575=ORIENTED_EDGE('',*,*,#2749,.F.);
#3576=ORIENTED_EDGE('',*,*,#2748,.F.);
#3577=ORIENTED_EDGE('',*,*,#2750,.T.);
#3578=ORIENTED_EDGE('',*,*,#2751,.T.);
#3579=ORIENTED_EDGE('',*,*,#2752,.T.);
#3580=ORIENTED_EDGE('',*,*,#2753,.T.);
#3581=ORIENTED_EDGE('',*,*,#2738,.T.);
#3582=ORIENTED_EDGE('',*,*,#2744,.T.);
#3583=ORIENTED_EDGE('',*,*,#2754,.F.);
#3584=ORIENTED_EDGE('',*,*,#2755,.T.);
#3585=ORIENTED_EDGE('',*,*,#2756,.T.);
#3586=ORIENTED_EDGE('',*,*,#2757,.T.);
#3587=ORIENTED_EDGE('',*,*,#2741,.T.);
#3588=ORIENTED_EDGE('',*,*,#2747,.T.);
#3589=ORIENTED_EDGE('',*,*,#2752,.F.);
#3590=ORIENTED_EDGE('',*,*,#2758,.T.);
#3591=ORIENTED_EDGE('',*,*,#2759,.F.);
#3592=ORIENTED_EDGE('',*,*,#2760,.F.);
#3593=ORIENTED_EDGE('',*,*,#2756,.F.);
#3594=ORIENTED_EDGE('',*,*,#2761,.T.);
#3595=ORIENTED_EDGE('',*,*,#2762,.F.);
#3596=ORIENTED_EDGE('',*,*,#2763,.F.);
#3597=ORIENTED_EDGE('',*,*,#2762,.T.);
#3598=ORIENTED_EDGE('',*,*,#2764,.T.);
#3599=ORIENTED_EDGE('',*,*,#2759,.T.);
#3600=ORIENTED_EDGE('',*,*,#2765,.T.);
#3601=ORIENTED_EDGE('',*,*,#2740,.T.);
#3602=ORIENTED_EDGE('',*,*,#2743,.T.);
#3603=ORIENTED_EDGE('',*,*,#2746,.T.);
#3604=ORIENTED_EDGE('',*,*,#2749,.T.);
#3605=ORIENTED_EDGE('',*,*,#2766,.F.);
#3606=ORIENTED_EDGE('',*,*,#2767,.T.);
#3607=ORIENTED_EDGE('',*,*,#2768,.F.);
#3608=ORIENTED_EDGE('',*,*,#2767,.F.);
#3609=ORIENTED_EDGE('',*,*,#2769,.T.);
#3610=ORIENTED_EDGE('',*,*,#2753,.F.);
#3611=ORIENTED_EDGE('',*,*,#2760,.T.);
#3612=ORIENTED_EDGE('',*,*,#2764,.F.);
#3613=ORIENTED_EDGE('',*,*,#2761,.F.);
#3614=ORIENTED_EDGE('',*,*,#2755,.F.);
#3615=ORIENTED_EDGE('',*,*,#2770,.F.);
#3616=ORIENTED_EDGE('',*,*,#2771,.F.);
#3617=ORIENTED_EDGE('',*,*,#2772,.T.);
#3618=ORIENTED_EDGE('',*,*,#2771,.T.);
#3619=ORIENTED_EDGE('',*,*,#2773,.F.);
#3620=ORIENTED_EDGE('',*,*,#2774,.F.);
#3621=ORIENTED_EDGE('',*,*,#2775,.T.);
#3622=ORIENTED_EDGE('',*,*,#2774,.T.);
#3623=ORIENTED_EDGE('',*,*,#2776,.F.);
#3624=ORIENTED_EDGE('',*,*,#2757,.F.);
#3625=ORIENTED_EDGE('',*,*,#2763,.T.);
#3626=ORIENTED_EDGE('',*,*,#2765,.F.);
#3627=ORIENTED_EDGE('',*,*,#2758,.F.);
#3628=ORIENTED_EDGE('',*,*,#2751,.F.);
#3629=ORIENTED_EDGE('',*,*,#2776,.T.);
#3630=ORIENTED_EDGE('',*,*,#2773,.T.);
#3631=ORIENTED_EDGE('',*,*,#2770,.T.);
#3632=ORIENTED_EDGE('',*,*,#2754,.T.);
#3633=ORIENTED_EDGE('',*,*,#2734,.T.);
#3634=ORIENTED_EDGE('',*,*,#2737,.T.);
#3635=ORIENTED_EDGE('',*,*,#2768,.T.);
#3636=ORIENTED_EDGE('',*,*,#2775,.F.);
#3637=ORIENTED_EDGE('',*,*,#2750,.F.);
#3638=ORIENTED_EDGE('',*,*,#2769,.F.);
#3639=ORIENTED_EDGE('',*,*,#2772,.F.);
#3640=ORIENTED_EDGE('',*,*,#2732,.T.);
#3641=ORIENTED_EDGE('',*,*,#2735,.T.);
#3642=ORIENTED_EDGE('',*,*,#2766,.T.);
#3643=ORIENTED_EDGE('',*,*,#2777,.T.);
#3644=ORIENTED_EDGE('',*,*,#2778,.T.);
#3645=ORIENTED_EDGE('',*,*,#2779,.T.);
#3646=ORIENTED_EDGE('',*,*,#2780,.T.);
#3647=ORIENTED_EDGE('',*,*,#2781,.T.);
#3648=ORIENTED_EDGE('',*,*,#2782,.T.);
#3649=ORIENTED_EDGE('',*,*,#2783,.F.);
#3650=ORIENTED_EDGE('',*,*,#2784,.T.);
#3651=ORIENTED_EDGE('',*,*,#2785,.T.);
#3652=ORIENTED_EDGE('',*,*,#2786,.T.);
#3653=ORIENTED_EDGE('',*,*,#2787,.T.);
#3654=ORIENTED_EDGE('',*,*,#2788,.T.);
#3655=ORIENTED_EDGE('',*,*,#2789,.T.);
#3656=ORIENTED_EDGE('',*,*,#2790,.F.);
#3657=ORIENTED_EDGE('',*,*,#2791,.F.);
#3658=ORIENTED_EDGE('',*,*,#2789,.F.);
#3659=ORIENTED_EDGE('',*,*,#2792,.F.);
#3660=ORIENTED_EDGE('',*,*,#2778,.F.);
#3661=ORIENTED_EDGE('',*,*,#2792,.T.);
#3662=ORIENTED_EDGE('',*,*,#2788,.F.);
#3663=ORIENTED_EDGE('',*,*,#2793,.F.);
#3664=ORIENTED_EDGE('',*,*,#2779,.F.);
#3665=ORIENTED_EDGE('',*,*,#2793,.T.);
#3666=ORIENTED_EDGE('',*,*,#2787,.F.);
#3667=ORIENTED_EDGE('',*,*,#2794,.F.);
#3668=ORIENTED_EDGE('',*,*,#2780,.F.);
#3669=ORIENTED_EDGE('',*,*,#2794,.T.);
#3670=ORIENTED_EDGE('',*,*,#2786,.F.);
#3671=ORIENTED_EDGE('',*,*,#2795,.F.);
#3672=ORIENTED_EDGE('',*,*,#2781,.F.);
#3673=ORIENTED_EDGE('',*,*,#2795,.T.);
#3674=ORIENTED_EDGE('',*,*,#2785,.F.);
#3675=ORIENTED_EDGE('',*,*,#2796,.F.);
#3676=ORIENTED_EDGE('',*,*,#2782,.F.);
#3677=ORIENTED_EDGE('',*,*,#2796,.T.);
#3678=ORIENTED_EDGE('',*,*,#2784,.F.);
#3679=ORIENTED_EDGE('',*,*,#2791,.T.);
#3680=ORIENTED_EDGE('',*,*,#2777,.F.);
#3681=ORIENTED_EDGE('',*,*,#2790,.T.);
#3682=ORIENTED_EDGE('',*,*,#2797,.T.);
#3683=ORIENTED_EDGE('',*,*,#2798,.T.);
#3684=ORIENTED_EDGE('',*,*,#2797,.F.);
#3685=ORIENTED_EDGE('',*,*,#2799,.F.);
#3686=ORIENTED_EDGE('',*,*,#2800,.T.);
#3687=ORIENTED_EDGE('',*,*,#2798,.F.);
#3688=ORIENTED_EDGE('',*,*,#2801,.T.);
#3689=ORIENTED_EDGE('',*,*,#2799,.T.);
#3690=ORIENTED_EDGE('',*,*,#2801,.F.);
#3691=ORIENTED_EDGE('',*,*,#2802,.F.);
#3692=ORIENTED_EDGE('',*,*,#2803,.T.);
#3693=ORIENTED_EDGE('',*,*,#2783,.T.);
#3694=ORIENTED_EDGE('',*,*,#2803,.F.);
#3695=ORIENTED_EDGE('',*,*,#2804,.F.);
#3696=ORIENTED_EDGE('',*,*,#2805,.T.);
#3697=ORIENTED_EDGE('',*,*,#2802,.T.);
#3698=ORIENTED_EDGE('',*,*,#2805,.F.);
#3699=ORIENTED_EDGE('',*,*,#2804,.T.);
#3700=ORIENTED_EDGE('',*,*,#2806,.F.);
#3701=ORIENTED_EDGE('',*,*,#2806,.T.);
#3702=ORIENTED_EDGE('',*,*,#2807,.T.);
#3703=ORIENTED_EDGE('',*,*,#2800,.F.);
#3704=ORIENTED_EDGE('',*,*,#2807,.F.);
#3705=ORIENTED_EDGE('',*,*,#2808,.F.);
#3706=ORIENTED_EDGE('',*,*,#2809,.T.);
#3707=ORIENTED_EDGE('',*,*,#2810,.T.);
#3708=ORIENTED_EDGE('',*,*,#2809,.F.);
#3709=ORIENTED_EDGE('',*,*,#2811,.F.);
#3710=ORIENTED_EDGE('',*,*,#2812,.T.);
#3711=ORIENTED_EDGE('',*,*,#2813,.T.);
#3712=ORIENTED_EDGE('',*,*,#2812,.F.);
#3713=ORIENTED_EDGE('',*,*,#2811,.T.);
#3714=ORIENTED_EDGE('',*,*,#2808,.T.);
#3715=ORIENTED_EDGE('',*,*,#2813,.F.);
#3716=ORIENTED_EDGE('',*,*,#2810,.F.);
#3717=ORIENTED_EDGE('',*,*,#2814,.F.);
#3718=ORIENTED_EDGE('',*,*,#2815,.F.);
#3719=ORIENTED_EDGE('',*,*,#2816,.F.);
#3720=ORIENTED_EDGE('',*,*,#2817,.T.);
#3721=ORIENTED_EDGE('',*,*,#2814,.T.);
#3722=ORIENTED_EDGE('',*,*,#2817,.F.);
#3723=ORIENTED_EDGE('',*,*,#2818,.T.);
#3724=ORIENTED_EDGE('',*,*,#2819,.F.);
#3725=ORIENTED_EDGE('',*,*,#2820,.F.);
#3726=ORIENTED_EDGE('',*,*,#2821,.F.);
#3727=ORIENTED_EDGE('',*,*,#2818,.F.);
#3728=ORIENTED_EDGE('',*,*,#2822,.T.);
#3729=ORIENTED_EDGE('',*,*,#2820,.T.);
#3730=ORIENTED_EDGE('',*,*,#2822,.F.);
#3731=ORIENTED_EDGE('',*,*,#2821,.T.);
#3732=ORIENTED_EDGE('',*,*,#2823,.T.);
#3733=ORIENTED_EDGE('',*,*,#2824,.F.);
#3734=ORIENTED_EDGE('',*,*,#2823,.F.);
#3735=ORIENTED_EDGE('',*,*,#2815,.T.);
#3736=ORIENTED_EDGE('',*,*,#2825,.T.);
#3737=ORIENTED_EDGE('',*,*,#2819,.T.);
#3738=ORIENTED_EDGE('',*,*,#2825,.F.);
#3739=ORIENTED_EDGE('',*,*,#2816,.T.);
#3740=ORIENTED_EDGE('',*,*,#2826,.F.);
#3741=ORIENTED_EDGE('',*,*,#2827,.T.);
#3742=ORIENTED_EDGE('',*,*,#2828,.T.);
#3743=ORIENTED_EDGE('',*,*,#2827,.F.);
#3744=ORIENTED_EDGE('',*,*,#2826,.T.);
#3745=ORIENTED_EDGE('',*,*,#2824,.T.);
#3746=ORIENTED_EDGE('',*,*,#2828,.F.);
#3747=ORIENTED_EDGE('',*,*,#2829,.F.);
#3748=ORIENTED_EDGE('',*,*,#2830,.T.);
#3749=ORIENTED_EDGE('',*,*,#2831,.T.);
#3750=ORIENTED_EDGE('',*,*,#2830,.F.);
#3751=ORIENTED_EDGE('',*,*,#2832,.F.);
#3752=ORIENTED_EDGE('',*,*,#2833,.T.);
#3753=ORIENTED_EDGE('',*,*,#2834,.T.);
#3754=ORIENTED_EDGE('',*,*,#2833,.F.);
#3755=ORIENTED_EDGE('',*,*,#2832,.T.);
#3756=ORIENTED_EDGE('',*,*,#2829,.T.);
#3757=ORIENTED_EDGE('',*,*,#2834,.F.);
#3758=ORIENTED_EDGE('',*,*,#2831,.F.);
#3759=ORIENTED_EDGE('',*,*,#2835,.F.);
#3760=ORIENTED_EDGE('',*,*,#2836,.T.);
#3761=ORIENTED_EDGE('',*,*,#2837,.F.);
#3762=ORIENTED_EDGE('',*,*,#2836,.F.);
#3763=ORIENTED_EDGE('',*,*,#2838,.F.);
#3764=ORIENTED_EDGE('',*,*,#2839,.T.);
#3765=ORIENTED_EDGE('',*,*,#2840,.F.);
#3766=ORIENTED_EDGE('',*,*,#2839,.F.);
#3767=ORIENTED_EDGE('',*,*,#2841,.F.);
#3768=ORIENTED_EDGE('',*,*,#2842,.T.);
#3769=ORIENTED_EDGE('',*,*,#2843,.F.);
#3770=ORIENTED_EDGE('',*,*,#2842,.F.);
#3771=ORIENTED_EDGE('',*,*,#2844,.F.);
#3772=ORIENTED_EDGE('',*,*,#2845,.T.);
#3773=ORIENTED_EDGE('',*,*,#2846,.F.);
#3774=ORIENTED_EDGE('',*,*,#2845,.F.);
#3775=ORIENTED_EDGE('',*,*,#2847,.F.);
#3776=ORIENTED_EDGE('',*,*,#2848,.T.);
#3777=ORIENTED_EDGE('',*,*,#2849,.F.);
#3778=ORIENTED_EDGE('',*,*,#2848,.F.);
#3779=ORIENTED_EDGE('',*,*,#2850,.F.);
#3780=ORIENTED_EDGE('',*,*,#2851,.T.);
#3781=ORIENTED_EDGE('',*,*,#2852,.F.);
#3782=ORIENTED_EDGE('',*,*,#2851,.F.);
#3783=ORIENTED_EDGE('',*,*,#2853,.F.);
#3784=ORIENTED_EDGE('',*,*,#2854,.T.);
#3785=ORIENTED_EDGE('',*,*,#2855,.T.);
#3786=ORIENTED_EDGE('',*,*,#2854,.F.);
#3787=ORIENTED_EDGE('',*,*,#2856,.F.);
#3788=ORIENTED_EDGE('',*,*,#2857,.T.);
#3789=ORIENTED_EDGE('',*,*,#2858,.T.);
#3790=ORIENTED_EDGE('',*,*,#2857,.F.);
#3791=ORIENTED_EDGE('',*,*,#2856,.T.);
#3792=ORIENTED_EDGE('',*,*,#2853,.T.);
#3793=ORIENTED_EDGE('',*,*,#2852,.T.);
#3794=ORIENTED_EDGE('',*,*,#2849,.T.);
#3795=ORIENTED_EDGE('',*,*,#2846,.T.);
#3796=ORIENTED_EDGE('',*,*,#2843,.T.);
#3797=ORIENTED_EDGE('',*,*,#2840,.T.);
#3798=ORIENTED_EDGE('',*,*,#2837,.T.);
#3799=ORIENTED_EDGE('',*,*,#2858,.F.);
#3800=ORIENTED_EDGE('',*,*,#2855,.F.);
#3801=ORIENTED_EDGE('',*,*,#2850,.T.);
#3802=ORIENTED_EDGE('',*,*,#2847,.T.);
#3803=ORIENTED_EDGE('',*,*,#2844,.T.);
#3804=ORIENTED_EDGE('',*,*,#2841,.T.);
#3805=ORIENTED_EDGE('',*,*,#2838,.T.);
#3806=ORIENTED_EDGE('',*,*,#2835,.T.);
#3807=ORIENTED_EDGE('',*,*,#2859,.F.);
#3808=ORIENTED_EDGE('',*,*,#2860,.T.);
#3809=ORIENTED_EDGE('',*,*,#2861,.F.);
#3810=ORIENTED_EDGE('',*,*,#2860,.F.);
#3811=ORIENTED_EDGE('',*,*,#2862,.F.);
#3812=ORIENTED_EDGE('',*,*,#2863,.T.);
#3813=ORIENTED_EDGE('',*,*,#2864,.F.);
#3814=ORIENTED_EDGE('',*,*,#2863,.F.);
#3815=ORIENTED_EDGE('',*,*,#2862,.T.);
#3816=ORIENTED_EDGE('',*,*,#2859,.T.);
#3817=ORIENTED_EDGE('',*,*,#2865,.T.);
#3818=ORIENTED_EDGE('',*,*,#2864,.T.);
#3819=ORIENTED_EDGE('',*,*,#2866,.F.);
#3820=ORIENTED_EDGE('',*,*,#2867,.T.);
#3821=ORIENTED_EDGE('',*,*,#2868,.T.);
#3822=ORIENTED_EDGE('',*,*,#2867,.F.);
#3823=ORIENTED_EDGE('',*,*,#2865,.F.);
#3824=ORIENTED_EDGE('',*,*,#2869,.T.);
#3825=ORIENTED_EDGE('',*,*,#2870,.T.);
#3826=ORIENTED_EDGE('',*,*,#2869,.F.);
#3827=ORIENTED_EDGE('',*,*,#2861,.T.);
#3828=ORIENTED_EDGE('',*,*,#2866,.T.);
#3829=ORIENTED_EDGE('',*,*,#2870,.F.);
#3830=ORIENTED_EDGE('',*,*,#2868,.F.);
#3831=ORIENTED_EDGE('',*,*,#2871,.F.);
#3832=ORIENTED_EDGE('',*,*,#2872,.F.);
#3833=ORIENTED_EDGE('',*,*,#2873,.F.);
#3834=ORIENTED_EDGE('',*,*,#2874,.F.);
#3835=ORIENTED_EDGE('',*,*,#2875,.F.);
#3836=ORIENTED_EDGE('',*,*,#2872,.T.);
#3837=ORIENTED_EDGE('',*,*,#2876,.F.);
#3838=ORIENTED_EDGE('',*,*,#2877,.T.);
#3839=ORIENTED_EDGE('',*,*,#2878,.F.);
#3840=ORIENTED_EDGE('',*,*,#2879,.F.);
#3841=ORIENTED_EDGE('',*,*,#2880,.F.);
#3842=ORIENTED_EDGE('',*,*,#2877,.F.);
#3843=ORIENTED_EDGE('',*,*,#2881,.F.);
#3844=ORIENTED_EDGE('',*,*,#2882,.F.);
#3845=ORIENTED_EDGE('',*,*,#2883,.F.);
#3846=ORIENTED_EDGE('',*,*,#2884,.F.);
#3847=ORIENTED_EDGE('',*,*,#2885,.F.);
#3848=ORIENTED_EDGE('',*,*,#2882,.T.);
#3849=ORIENTED_EDGE('',*,*,#2886,.F.);
#3850=ORIENTED_EDGE('',*,*,#2887,.F.);
#3851=ORIENTED_EDGE('',*,*,#2888,.F.);
#3852=ORIENTED_EDGE('',*,*,#2889,.F.);
#3853=ORIENTED_EDGE('',*,*,#2890,.F.);
#3854=ORIENTED_EDGE('',*,*,#2887,.T.);
#3855=ORIENTED_EDGE('',*,*,#2891,.F.);
#3856=ORIENTED_EDGE('',*,*,#2892,.F.);
#3857=ORIENTED_EDGE('',*,*,#2893,.F.);
#3858=ORIENTED_EDGE('',*,*,#2894,.F.);
#3859=ORIENTED_EDGE('',*,*,#2895,.F.);
#3860=ORIENTED_EDGE('',*,*,#2892,.T.);
#3861=ORIENTED_EDGE('',*,*,#2896,.F.);
#3862=ORIENTED_EDGE('',*,*,#2897,.T.);
#3863=ORIENTED_EDGE('',*,*,#2898,.F.);
#3864=ORIENTED_EDGE('',*,*,#2899,.F.);
#3865=ORIENTED_EDGE('',*,*,#2900,.F.);
#3866=ORIENTED_EDGE('',*,*,#2897,.F.);
#3867=ORIENTED_EDGE('',*,*,#2901,.F.);
#3868=ORIENTED_EDGE('',*,*,#2902,.T.);
#3869=ORIENTED_EDGE('',*,*,#2903,.F.);
#3870=ORIENTED_EDGE('',*,*,#2893,.T.);
#3871=ORIENTED_EDGE('',*,*,#2891,.T.);
#3872=ORIENTED_EDGE('',*,*,#2895,.T.);
#3873=ORIENTED_EDGE('',*,*,#2904,.F.);
#3874=ORIENTED_EDGE('',*,*,#2873,.T.);
#3875=ORIENTED_EDGE('',*,*,#2871,.T.);
#3876=ORIENTED_EDGE('',*,*,#2875,.T.);
#3877=ORIENTED_EDGE('',*,*,#2905,.F.);
#3878=ORIENTED_EDGE('',*,*,#2898,.T.);
#3879=ORIENTED_EDGE('',*,*,#2900,.T.);
#3880=ORIENTED_EDGE('',*,*,#2896,.T.);
#3881=ORIENTED_EDGE('',*,*,#2906,.F.);
#3882=ORIENTED_EDGE('',*,*,#2878,.T.);
#3883=ORIENTED_EDGE('',*,*,#2880,.T.);
#3884=ORIENTED_EDGE('',*,*,#2876,.T.);
#3885=ORIENTED_EDGE('',*,*,#2907,.F.);
#3886=ORIENTED_EDGE('',*,*,#2883,.T.);
#3887=ORIENTED_EDGE('',*,*,#2881,.T.);
#3888=ORIENTED_EDGE('',*,*,#2885,.T.);
#3889=ORIENTED_EDGE('',*,*,#2908,.F.);
#3890=ORIENTED_EDGE('',*,*,#2888,.T.);
#3891=ORIENTED_EDGE('',*,*,#2886,.T.);
#3892=ORIENTED_EDGE('',*,*,#2890,.T.);
#3893=ORIENTED_EDGE('',*,*,#2909,.F.);
#3894=ORIENTED_EDGE('',*,*,#2902,.F.);
#3895=ORIENTED_EDGE('',*,*,#2910,.F.);
#3896=ORIENTED_EDGE('',*,*,#2911,.T.);
#3897=ORIENTED_EDGE('',*,*,#2912,.F.);
#3898=ORIENTED_EDGE('',*,*,#2911,.F.);
#3899=ORIENTED_EDGE('',*,*,#2913,.F.);
#3900=ORIENTED_EDGE('',*,*,#2914,.T.);
#3901=ORIENTED_EDGE('',*,*,#2915,.F.);
#3902=ORIENTED_EDGE('',*,*,#2914,.F.);
#3903=ORIENTED_EDGE('',*,*,#2916,.F.);
#3904=ORIENTED_EDGE('',*,*,#2917,.T.);
#3905=ORIENTED_EDGE('',*,*,#2918,.F.);
#3906=ORIENTED_EDGE('',*,*,#2917,.F.);
#3907=ORIENTED_EDGE('',*,*,#2919,.F.);
#3908=ORIENTED_EDGE('',*,*,#2920,.T.);
#3909=ORIENTED_EDGE('',*,*,#2921,.F.);
#3910=ORIENTED_EDGE('',*,*,#2920,.F.);
#3911=ORIENTED_EDGE('',*,*,#2922,.F.);
#3912=ORIENTED_EDGE('',*,*,#2923,.T.);
#3913=ORIENTED_EDGE('',*,*,#2924,.F.);
#3914=ORIENTED_EDGE('',*,*,#2923,.F.);
#3915=ORIENTED_EDGE('',*,*,#2925,.F.);
#3916=ORIENTED_EDGE('',*,*,#2926,.T.);
#3917=ORIENTED_EDGE('',*,*,#2927,.F.);
#3918=ORIENTED_EDGE('',*,*,#2926,.F.);
#3919=ORIENTED_EDGE('',*,*,#2928,.F.);
#3920=ORIENTED_EDGE('',*,*,#2929,.T.);
#3921=ORIENTED_EDGE('',*,*,#2930,.F.);
#3922=ORIENTED_EDGE('',*,*,#2929,.F.);
#3923=ORIENTED_EDGE('',*,*,#2931,.F.);
#3924=ORIENTED_EDGE('',*,*,#2932,.T.);
#3925=ORIENTED_EDGE('',*,*,#2933,.T.);
#3926=ORIENTED_EDGE('',*,*,#2932,.F.);
#3927=ORIENTED_EDGE('',*,*,#2933,.F.);
#3928=ORIENTED_EDGE('',*,*,#2928,.T.);
#3929=ORIENTED_EDGE('',*,*,#2901,.T.);
#3930=ORIENTED_EDGE('',*,*,#2930,.T.);
#3931=ORIENTED_EDGE('',*,*,#2934,.F.);
#3932=ORIENTED_EDGE('',*,*,#2935,.T.);
#3933=ORIENTED_EDGE('',*,*,#2936,.T.);
#3934=ORIENTED_EDGE('',*,*,#2935,.F.);
#3935=ORIENTED_EDGE('',*,*,#2934,.T.);
#3936=ORIENTED_EDGE('',*,*,#2912,.T.);
#3937=ORIENTED_EDGE('',*,*,#2915,.T.);
#3938=ORIENTED_EDGE('',*,*,#2918,.T.);
#3939=ORIENTED_EDGE('',*,*,#2921,.T.);
#3940=ORIENTED_EDGE('',*,*,#2924,.T.);
#3941=ORIENTED_EDGE('',*,*,#2927,.T.);
#3942=ORIENTED_EDGE('',*,*,#2904,.T.);
#3943=ORIENTED_EDGE('',*,*,#2894,.T.);
#3944=ORIENTED_EDGE('',*,*,#2903,.T.);
#3945=ORIENTED_EDGE('',*,*,#2909,.T.);
#3946=ORIENTED_EDGE('',*,*,#2889,.T.);
#3947=ORIENTED_EDGE('',*,*,#2908,.T.);
#3948=ORIENTED_EDGE('',*,*,#2884,.T.);
#3949=ORIENTED_EDGE('',*,*,#2907,.T.);
#3950=ORIENTED_EDGE('',*,*,#2879,.T.);
#3951=ORIENTED_EDGE('',*,*,#2906,.T.);
#3952=ORIENTED_EDGE('',*,*,#2899,.T.);
#3953=ORIENTED_EDGE('',*,*,#2905,.T.);
#3954=ORIENTED_EDGE('',*,*,#2874,.T.);
#3955=ORIENTED_EDGE('',*,*,#2936,.F.);
#3956=ORIENTED_EDGE('',*,*,#2931,.T.);
#3957=ORIENTED_EDGE('',*,*,#2925,.T.);
#3958=ORIENTED_EDGE('',*,*,#2922,.T.);
#3959=ORIENTED_EDGE('',*,*,#2919,.T.);
#3960=ORIENTED_EDGE('',*,*,#2916,.T.);
#3961=ORIENTED_EDGE('',*,*,#2913,.T.);
#3962=ORIENTED_EDGE('',*,*,#2910,.T.);
#3963=ORIENTED_EDGE('',*,*,#2937,.T.);
#3964=ORIENTED_EDGE('',*,*,#2938,.T.);
#3965=ORIENTED_EDGE('',*,*,#2939,.F.);
#3966=ORIENTED_EDGE('',*,*,#2938,.F.);
#3967=ORIENTED_EDGE('',*,*,#2939,.T.);
#3968=ORIENTED_EDGE('',*,*,#2937,.F.);
#3969=ORIENTED_EDGE('',*,*,#2940,.F.);
#3970=ORIENTED_EDGE('',*,*,#2941,.T.);
#3971=ORIENTED_EDGE('',*,*,#2942,.T.);
#3972=ORIENTED_EDGE('',*,*,#2941,.F.);
#3973=ORIENTED_EDGE('',*,*,#2942,.F.);
#3974=ORIENTED_EDGE('',*,*,#2943,.F.);
#3975=ORIENTED_EDGE('',*,*,#2944,.T.);
#3976=ORIENTED_EDGE('',*,*,#2945,.T.);
#3977=ORIENTED_EDGE('',*,*,#2944,.F.);
#3978=ORIENTED_EDGE('',*,*,#2943,.T.);
#3979=ORIENTED_EDGE('',*,*,#2945,.F.);
#3980=ORIENTED_EDGE('',*,*,#2940,.T.);
#3981=ORIENTED_EDGE('',*,*,#2946,.F.);
#3982=ORIENTED_EDGE('',*,*,#2947,.T.);
#3983=ORIENTED_EDGE('',*,*,#2948,.T.);
#3984=ORIENTED_EDGE('',*,*,#2947,.F.);
#3985=ORIENTED_EDGE('',*,*,#2946,.T.);
#3986=ORIENTED_EDGE('',*,*,#2948,.F.);
#3987=ORIENTED_EDGE('',*,*,#2949,.F.);
#3988=ORIENTED_EDGE('',*,*,#2950,.T.);
#3989=ORIENTED_EDGE('',*,*,#2951,.T.);
#3990=ORIENTED_EDGE('',*,*,#2952,.F.);
#3991=ORIENTED_EDGE('',*,*,#2953,.F.);
#3992=ORIENTED_EDGE('',*,*,#2954,.F.);
#3993=ORIENTED_EDGE('',*,*,#2951,.F.);
#3994=ORIENTED_EDGE('',*,*,#2955,.T.);
#3995=ORIENTED_EDGE('',*,*,#2956,.F.);
#3996=ORIENTED_EDGE('',*,*,#2955,.F.);
#3997=ORIENTED_EDGE('',*,*,#2950,.F.);
#3998=ORIENTED_EDGE('',*,*,#2957,.F.);
#3999=ORIENTED_EDGE('',*,*,#2953,.T.);
#4000=ORIENTED_EDGE('',*,*,#2958,.F.);
#4001=ORIENTED_EDGE('',*,*,#2959,.T.);
#4002=ORIENTED_EDGE('',*,*,#2960,.T.);
#4003=ORIENTED_EDGE('',*,*,#2959,.F.);
#4004=ORIENTED_EDGE('',*,*,#2954,.T.);
#4005=ORIENTED_EDGE('',*,*,#2957,.T.);
#4006=ORIENTED_EDGE('',*,*,#2952,.T.);
#4007=ORIENTED_EDGE('',*,*,#2949,.T.);
#4008=ORIENTED_EDGE('',*,*,#2961,.F.);
#4009=ORIENTED_EDGE('',*,*,#2962,.T.);
#4010=ORIENTED_EDGE('',*,*,#2963,.T.);
#4011=ORIENTED_EDGE('',*,*,#2962,.F.);
#4012=ORIENTED_EDGE('',*,*,#2956,.T.);
#4013=ORIENTED_EDGE('',*,*,#2961,.T.);
#4014=ORIENTED_EDGE('',*,*,#2958,.T.);
#4015=ORIENTED_EDGE('',*,*,#2963,.F.);
#4016=ORIENTED_EDGE('',*,*,#2960,.F.);
#4017=ORIENTED_EDGE('',*,*,#2964,.F.);
#4018=ORIENTED_EDGE('',*,*,#2965,.F.);
#4019=ORIENTED_EDGE('',*,*,#2966,.T.);
#4020=ORIENTED_EDGE('',*,*,#2964,.T.);
#4021=ORIENTED_EDGE('',*,*,#2966,.F.);
#4022=ORIENTED_EDGE('',*,*,#2967,.F.);
#4023=ORIENTED_EDGE('',*,*,#2968,.T.);
#4024=ORIENTED_EDGE('',*,*,#2965,.T.);
#4025=ORIENTED_EDGE('',*,*,#2968,.F.);
#4026=ORIENTED_EDGE('',*,*,#2969,.F.);
#4027=ORIENTED_EDGE('',*,*,#2970,.T.);
#4028=ORIENTED_EDGE('',*,*,#2967,.T.);
#4029=ORIENTED_EDGE('',*,*,#2970,.F.);
#4030=ORIENTED_EDGE('',*,*,#2969,.T.);
#4031=ORIENTED_EDGE('',*,*,#2971,.F.);
#4032=ORIENTED_EDGE('',*,*,#2972,.F.);
#4033=ORIENTED_EDGE('',*,*,#2973,.T.);
#4034=ORIENTED_EDGE('',*,*,#2971,.T.);
#4035=ORIENTED_EDGE('',*,*,#2973,.F.);
#4036=ORIENTED_EDGE('',*,*,#2974,.F.);
#4037=ORIENTED_EDGE('',*,*,#2975,.T.);
#4038=ORIENTED_EDGE('',*,*,#2972,.T.);
#4039=ORIENTED_EDGE('',*,*,#2975,.F.);
#4040=ORIENTED_EDGE('',*,*,#2976,.F.);
#4041=ORIENTED_EDGE('',*,*,#2977,.T.);
#4042=ORIENTED_EDGE('',*,*,#2974,.T.);
#4043=ORIENTED_EDGE('',*,*,#2977,.F.);
#4044=ORIENTED_EDGE('',*,*,#2976,.T.);
#4045=ORIENTED_EDGE('',*,*,#2978,.T.);
#4046=ORIENTED_EDGE('',*,*,#2979,.T.);
#4047=ORIENTED_EDGE('',*,*,#2980,.T.);
#4048=ORIENTED_EDGE('',*,*,#2981,.F.);
#4049=ORIENTED_EDGE('',*,*,#2982,.T.);
#4050=ORIENTED_EDGE('',*,*,#2983,.T.);
#4051=ORIENTED_EDGE('',*,*,#2984,.T.);
#4052=ORIENTED_EDGE('',*,*,#2979,.F.);
#4053=ORIENTED_EDGE('',*,*,#2985,.T.);
#4054=ORIENTED_EDGE('',*,*,#2986,.T.);
#4055=ORIENTED_EDGE('',*,*,#2987,.T.);
#4056=ORIENTED_EDGE('',*,*,#2983,.F.);
#4057=ORIENTED_EDGE('',*,*,#2988,.T.);
#4058=ORIENTED_EDGE('',*,*,#2989,.T.);
#4059=ORIENTED_EDGE('',*,*,#2990,.T.);
#4060=ORIENTED_EDGE('',*,*,#2986,.F.);
#4061=ORIENTED_EDGE('',*,*,#2991,.T.);
#4062=ORIENTED_EDGE('',*,*,#2992,.T.);
#4063=ORIENTED_EDGE('',*,*,#2993,.T.);
#4064=ORIENTED_EDGE('',*,*,#2989,.F.);
#4065=ORIENTED_EDGE('',*,*,#2994,.T.);
#4066=ORIENTED_EDGE('',*,*,#2981,.T.);
#4067=ORIENTED_EDGE('',*,*,#2995,.T.);
#4068=ORIENTED_EDGE('',*,*,#2992,.F.);
#4069=ORIENTED_EDGE('',*,*,#2994,.F.);
#4070=ORIENTED_EDGE('',*,*,#2991,.F.);
#4071=ORIENTED_EDGE('',*,*,#2988,.F.);
#4072=ORIENTED_EDGE('',*,*,#2985,.F.);
#4073=ORIENTED_EDGE('',*,*,#2982,.F.);
#4074=ORIENTED_EDGE('',*,*,#2978,.F.);
#4075=ORIENTED_EDGE('',*,*,#2995,.F.);
#4076=ORIENTED_EDGE('',*,*,#2980,.F.);
#4077=ORIENTED_EDGE('',*,*,#2984,.F.);
#4078=ORIENTED_EDGE('',*,*,#2987,.F.);
#4079=ORIENTED_EDGE('',*,*,#2990,.F.);
#4080=ORIENTED_EDGE('',*,*,#2993,.F.);
#4081=ORIENTED_EDGE('',*,*,#2996,.F.);
#4082=ORIENTED_EDGE('',*,*,#2997,.T.);
#4083=ORIENTED_EDGE('',*,*,#2998,.T.);
#4084=ORIENTED_EDGE('',*,*,#2997,.F.);
#4085=ORIENTED_EDGE('',*,*,#2999,.F.);
#4086=ORIENTED_EDGE('',*,*,#3000,.T.);
#4087=ORIENTED_EDGE('',*,*,#3001,.T.);
#4088=ORIENTED_EDGE('',*,*,#3000,.F.);
#4089=ORIENTED_EDGE('',*,*,#2999,.T.);
#4090=ORIENTED_EDGE('',*,*,#2996,.T.);
#4091=ORIENTED_EDGE('',*,*,#3001,.F.);
#4092=ORIENTED_EDGE('',*,*,#2998,.F.);
#4093=ORIENTED_EDGE('',*,*,#3002,.F.);
#4094=ORIENTED_EDGE('',*,*,#3003,.F.);
#4095=ORIENTED_EDGE('',*,*,#3004,.T.);
#4096=ORIENTED_EDGE('',*,*,#3005,.F.);
#4097=ORIENTED_EDGE('',*,*,#3004,.F.);
#4098=ORIENTED_EDGE('',*,*,#3006,.F.);
#4099=ORIENTED_EDGE('',*,*,#3007,.F.);
#4100=ORIENTED_EDGE('',*,*,#3008,.F.);
#4101=ORIENTED_EDGE('',*,*,#3009,.F.);
#4102=ORIENTED_EDGE('',*,*,#3010,.F.);
#4103=ORIENTED_EDGE('',*,*,#3011,.T.);
#4104=ORIENTED_EDGE('',*,*,#3012,.F.);
#4105=ORIENTED_EDGE('',*,*,#3013,.F.);
#4106=ORIENTED_EDGE('',*,*,#3014,.F.);
#4107=ORIENTED_EDGE('',*,*,#3015,.F.);
#4108=ORIENTED_EDGE('',*,*,#3016,.F.);
#4109=ORIENTED_EDGE('',*,*,#3017,.F.);
#4110=ORIENTED_EDGE('',*,*,#3011,.F.);
#4111=ORIENTED_EDGE('',*,*,#3007,.T.);
#4112=ORIENTED_EDGE('',*,*,#3018,.T.);
#4113=ORIENTED_EDGE('',*,*,#3016,.T.);
#4114=ORIENTED_EDGE('',*,*,#3019,.F.);
#4115=ORIENTED_EDGE('',*,*,#3006,.T.);
#4116=ORIENTED_EDGE('',*,*,#3020,.T.);
#4117=ORIENTED_EDGE('',*,*,#3017,.T.);
#4118=ORIENTED_EDGE('',*,*,#3018,.F.);
#4119=ORIENTED_EDGE('',*,*,#3003,.T.);
#4120=ORIENTED_EDGE('',*,*,#3021,.T.);
#4121=ORIENTED_EDGE('',*,*,#3012,.T.);
#4122=ORIENTED_EDGE('',*,*,#3020,.F.);
#4123=ORIENTED_EDGE('',*,*,#3022,.F.);
#4124=ORIENTED_EDGE('',*,*,#3023,.T.);
#4125=ORIENTED_EDGE('',*,*,#3024,.T.);
#4126=ORIENTED_EDGE('',*,*,#3023,.F.);
#4127=ORIENTED_EDGE('',*,*,#3002,.T.);
#4128=ORIENTED_EDGE('',*,*,#3025,.T.);
#4129=ORIENTED_EDGE('',*,*,#3013,.T.);
#4130=ORIENTED_EDGE('',*,*,#3021,.F.);
#4131=ORIENTED_EDGE('',*,*,#3008,.T.);
#4132=ORIENTED_EDGE('',*,*,#3019,.T.);
#4133=ORIENTED_EDGE('',*,*,#3015,.T.);
#4134=ORIENTED_EDGE('',*,*,#3026,.F.);
#4135=ORIENTED_EDGE('',*,*,#3009,.T.);
#4136=ORIENTED_EDGE('',*,*,#3026,.T.);
#4137=ORIENTED_EDGE('',*,*,#3014,.T.);
#4138=ORIENTED_EDGE('',*,*,#3025,.F.);
#4139=ORIENTED_EDGE('',*,*,#3010,.T.);
#4140=ORIENTED_EDGE('',*,*,#3022,.T.);
#4141=ORIENTED_EDGE('',*,*,#3005,.T.);
#4142=ORIENTED_EDGE('',*,*,#3024,.F.);
#4143=ORIENTED_EDGE('',*,*,#3027,.F.);
#4144=ORIENTED_EDGE('',*,*,#3028,.T.);
#4145=ORIENTED_EDGE('',*,*,#3029,.T.);
#4146=ORIENTED_EDGE('',*,*,#3030,.F.);
#4147=ORIENTED_EDGE('',*,*,#3031,.F.);
#4148=ORIENTED_EDGE('',*,*,#3032,.T.);
#4149=ORIENTED_EDGE('',*,*,#3033,.T.);
#4150=ORIENTED_EDGE('',*,*,#3028,.F.);
#4151=ORIENTED_EDGE('',*,*,#3034,.F.);
#4152=ORIENTED_EDGE('',*,*,#3035,.T.);
#4153=ORIENTED_EDGE('',*,*,#3036,.T.);
#4154=ORIENTED_EDGE('',*,*,#3032,.F.);
#4155=ORIENTED_EDGE('',*,*,#3037,.F.);
#4156=ORIENTED_EDGE('',*,*,#3038,.T.);
#4157=ORIENTED_EDGE('',*,*,#3039,.T.);
#4158=ORIENTED_EDGE('',*,*,#3035,.F.);
#4159=ORIENTED_EDGE('',*,*,#3040,.F.);
#4160=ORIENTED_EDGE('',*,*,#3041,.T.);
#4161=ORIENTED_EDGE('',*,*,#3042,.T.);
#4162=ORIENTED_EDGE('',*,*,#3038,.F.);
#4163=ORIENTED_EDGE('',*,*,#3043,.F.);
#4164=ORIENTED_EDGE('',*,*,#3030,.T.);
#4165=ORIENTED_EDGE('',*,*,#3044,.T.);
#4166=ORIENTED_EDGE('',*,*,#3041,.F.);
#4167=ORIENTED_EDGE('',*,*,#3044,.F.);
#4168=ORIENTED_EDGE('',*,*,#3029,.F.);
#4169=ORIENTED_EDGE('',*,*,#3033,.F.);
#4170=ORIENTED_EDGE('',*,*,#3036,.F.);
#4171=ORIENTED_EDGE('',*,*,#3039,.F.);
#4172=ORIENTED_EDGE('',*,*,#3042,.F.);
#4173=ORIENTED_EDGE('',*,*,#3045,.F.);
#4174=ORIENTED_EDGE('',*,*,#3027,.T.);
#4175=ORIENTED_EDGE('',*,*,#3043,.T.);
#4176=ORIENTED_EDGE('',*,*,#3040,.T.);
#4177=ORIENTED_EDGE('',*,*,#3037,.T.);
#4178=ORIENTED_EDGE('',*,*,#3034,.T.);
#4179=ORIENTED_EDGE('',*,*,#3031,.T.);
#4180=ORIENTED_EDGE('',*,*,#3046,.F.);
#4181=ORIENTED_EDGE('',*,*,#3047,.T.);
#4182=ORIENTED_EDGE('',*,*,#3045,.T.);
#4183=ORIENTED_EDGE('',*,*,#3047,.F.);
#4184=ORIENTED_EDGE('',*,*,#3048,.F.);
#4185=ORIENTED_EDGE('',*,*,#3049,.T.);
#4186=ORIENTED_EDGE('',*,*,#3046,.T.);
#4187=ORIENTED_EDGE('',*,*,#3049,.F.);
#4188=ORIENTED_EDGE('',*,*,#3050,.F.);
#4189=ORIENTED_EDGE('',*,*,#3051,.T.);
#4190=ORIENTED_EDGE('',*,*,#3048,.T.);
#4191=ORIENTED_EDGE('',*,*,#3051,.F.);
#4192=ORIENTED_EDGE('',*,*,#3050,.T.);
#4193=ORIENTED_EDGE('',*,*,#3052,.F.);
#4194=ORIENTED_EDGE('',*,*,#3053,.T.);
#4195=ORIENTED_EDGE('',*,*,#3052,.T.);
#4196=ORIENTED_EDGE('',*,*,#3053,.F.);
#4197=ORIENTED_EDGE('',*,*,#3054,.F.);
#4198=ORIENTED_EDGE('',*,*,#3055,.T.);
#4199=ORIENTED_EDGE('',*,*,#3056,.F.);
#4200=ORIENTED_EDGE('',*,*,#3055,.F.);
#4201=ORIENTED_EDGE('',*,*,#3057,.T.);
#4202=ORIENTED_EDGE('',*,*,#3058,.T.);
#4203=ORIENTED_EDGE('',*,*,#3059,.F.);
#4204=ORIENTED_EDGE('',*,*,#3060,.F.);
#4205=ORIENTED_EDGE('',*,*,#3061,.T.);
#4206=ORIENTED_EDGE('',*,*,#3060,.T.);
#4207=ORIENTED_EDGE('',*,*,#3062,.F.);
#4208=ORIENTED_EDGE('',*,*,#3063,.F.);
#4209=ORIENTED_EDGE('',*,*,#3064,.T.);
#4210=ORIENTED_EDGE('',*,*,#3063,.T.);
#4211=ORIENTED_EDGE('',*,*,#3065,.F.);
#4212=ORIENTED_EDGE('',*,*,#3066,.F.);
#4213=ORIENTED_EDGE('',*,*,#3067,.T.);
#4214=ORIENTED_EDGE('',*,*,#3066,.T.);
#4215=ORIENTED_EDGE('',*,*,#3068,.F.);
#4216=ORIENTED_EDGE('',*,*,#3058,.F.);
#4217=ORIENTED_EDGE('',*,*,#3068,.T.);
#4218=ORIENTED_EDGE('',*,*,#3065,.T.);
#4219=ORIENTED_EDGE('',*,*,#3062,.T.);
#4220=ORIENTED_EDGE('',*,*,#3059,.T.);
#4221=ORIENTED_EDGE('',*,*,#3056,.T.);
#4222=ORIENTED_EDGE('',*,*,#3067,.F.);
#4223=ORIENTED_EDGE('',*,*,#3057,.F.);
#4224=ORIENTED_EDGE('',*,*,#3061,.F.);
#4225=ORIENTED_EDGE('',*,*,#3064,.F.);
#4226=ORIENTED_EDGE('',*,*,#3054,.T.);
#4227=ORIENTED_EDGE('',*,*,#3069,.F.);
#4228=ORIENTED_EDGE('',*,*,#3070,.F.);
#4229=ORIENTED_EDGE('',*,*,#3071,.T.);
#4230=ORIENTED_EDGE('',*,*,#3069,.T.);
#4231=ORIENTED_EDGE('',*,*,#3071,.F.);
#4232=ORIENTED_EDGE('',*,*,#3072,.F.);
#4233=ORIENTED_EDGE('',*,*,#3073,.T.);
#4234=ORIENTED_EDGE('',*,*,#3070,.T.);
#4235=ORIENTED_EDGE('',*,*,#3073,.F.);
#4236=ORIENTED_EDGE('',*,*,#3074,.F.);
#4237=ORIENTED_EDGE('',*,*,#3075,.T.);
#4238=ORIENTED_EDGE('',*,*,#3072,.T.);
#4239=ORIENTED_EDGE('',*,*,#3075,.F.);
#4240=ORIENTED_EDGE('',*,*,#3074,.T.);
#4241=ORIENTED_EDGE('',*,*,#3076,.F.);
#4242=ORIENTED_EDGE('',*,*,#3077,.F.);
#4243=ORIENTED_EDGE('',*,*,#3078,.T.);
#4244=ORIENTED_EDGE('',*,*,#3076,.T.);
#4245=ORIENTED_EDGE('',*,*,#3078,.F.);
#4246=ORIENTED_EDGE('',*,*,#3079,.F.);
#4247=ORIENTED_EDGE('',*,*,#3080,.T.);
#4248=ORIENTED_EDGE('',*,*,#3077,.T.);
#4249=ORIENTED_EDGE('',*,*,#3080,.F.);
#4250=ORIENTED_EDGE('',*,*,#3081,.F.);
#4251=ORIENTED_EDGE('',*,*,#3082,.T.);
#4252=ORIENTED_EDGE('',*,*,#3079,.T.);
#4253=ORIENTED_EDGE('',*,*,#3082,.F.);
#4254=ORIENTED_EDGE('',*,*,#3081,.T.);
#4255=ORIENTED_EDGE('',*,*,#3083,.T.);
#4256=ORIENTED_EDGE('',*,*,#3084,.T.);
#4257=ORIENTED_EDGE('',*,*,#3085,.T.);
#4258=ORIENTED_EDGE('',*,*,#3086,.F.);
#4259=ORIENTED_EDGE('',*,*,#3087,.T.);
#4260=ORIENTED_EDGE('',*,*,#3088,.T.);
#4261=ORIENTED_EDGE('',*,*,#3089,.T.);
#4262=ORIENTED_EDGE('',*,*,#3084,.F.);
#4263=ORIENTED_EDGE('',*,*,#3090,.T.);
#4264=ORIENTED_EDGE('',*,*,#3091,.T.);
#4265=ORIENTED_EDGE('',*,*,#3092,.T.);
#4266=ORIENTED_EDGE('',*,*,#3088,.F.);
#4267=ORIENTED_EDGE('',*,*,#3093,.T.);
#4268=ORIENTED_EDGE('',*,*,#3094,.T.);
#4269=ORIENTED_EDGE('',*,*,#3095,.T.);
#4270=ORIENTED_EDGE('',*,*,#3091,.F.);
#4271=ORIENTED_EDGE('',*,*,#3096,.T.);
#4272=ORIENTED_EDGE('',*,*,#3097,.T.);
#4273=ORIENTED_EDGE('',*,*,#3098,.T.);
#4274=ORIENTED_EDGE('',*,*,#3094,.F.);
#4275=ORIENTED_EDGE('',*,*,#3099,.T.);
#4276=ORIENTED_EDGE('',*,*,#3086,.T.);
#4277=ORIENTED_EDGE('',*,*,#3100,.T.);
#4278=ORIENTED_EDGE('',*,*,#3097,.F.);
#4279=ORIENTED_EDGE('',*,*,#3099,.F.);
#4280=ORIENTED_EDGE('',*,*,#3096,.F.);
#4281=ORIENTED_EDGE('',*,*,#3093,.F.);
#4282=ORIENTED_EDGE('',*,*,#3090,.F.);
#4283=ORIENTED_EDGE('',*,*,#3087,.F.);
#4284=ORIENTED_EDGE('',*,*,#3083,.F.);
#4285=ORIENTED_EDGE('',*,*,#3100,.F.);
#4286=ORIENTED_EDGE('',*,*,#3085,.F.);
#4287=ORIENTED_EDGE('',*,*,#3089,.F.);
#4288=ORIENTED_EDGE('',*,*,#3092,.F.);
#4289=ORIENTED_EDGE('',*,*,#3095,.F.);
#4290=ORIENTED_EDGE('',*,*,#3098,.F.);
#4291=CYLINDRICAL_SURFACE('',#4972,0.165);
#4292=CYLINDRICAL_SURFACE('',#4974,0.165);
#4293=CYLINDRICAL_SURFACE('',#4978,0.165);
#4294=CYLINDRICAL_SURFACE('',#4982,0.165);
#4295=CYLINDRICAL_SURFACE('',#4986,0.165);
#4296=CYLINDRICAL_SURFACE('',#4990,0.165);
#4297=CYLINDRICAL_SURFACE('',#4994,2.24);
#4298=CYLINDRICAL_SURFACE('',#4997,2.46);
#4299=CYLINDRICAL_SURFACE('',#5006,0.21);
#4300=CYLINDRICAL_SURFACE('',#5008,0.21);
#4301=CYLINDRICAL_SURFACE('',#5012,0.21);
#4302=CYLINDRICAL_SURFACE('',#5016,0.21);
#4303=CYLINDRICAL_SURFACE('',#5020,0.21);
#4304=CYLINDRICAL_SURFACE('',#5024,0.21);
#4305=CYLINDRICAL_SURFACE('',#5036,0.2);
#4306=CYLINDRICAL_SURFACE('',#5039,0.2);
#4307=CYLINDRICAL_SURFACE('',#5042,0.2);
#4308=CYLINDRICAL_SURFACE('',#5046,0.2);
#4309=CYLINDRICAL_SURFACE('',#5047,0.685);
#4310=CYLINDRICAL_SURFACE('',#5048,0.4);
#4311=CYLINDRICAL_SURFACE('',#5050,0.685);
#4312=CYLINDRICAL_SURFACE('',#5059,0.4);
#4313=CYLINDRICAL_SURFACE('',#5062,0.4);
#4314=CYLINDRICAL_SURFACE('',#5065,0.4);
#4315=CYLINDRICAL_SURFACE('',#5074,0.4);
#4316=CYLINDRICAL_SURFACE('',#5076,0.685);
#4317=CYLINDRICAL_SURFACE('',#5079,0.89);
#4318=CYLINDRICAL_SURFACE('',#5086,0.6185);
#4319=CYLINDRICAL_SURFACE('',#5088,0.6185);
#4320=CYLINDRICAL_SURFACE('',#5090,1.1);
#4321=CYLINDRICAL_SURFACE('',#5096,0.6);
#4322=CYLINDRICAL_SURFACE('',#5099,0.8);
#4323=CYLINDRICAL_SURFACE('',#5102,2.5);
#4324=CYLINDRICAL_SURFACE('',#5106,3.31);
#4325=CYLINDRICAL_SURFACE('',#5109,4.5);
#4326=CYLINDRICAL_SURFACE('',#5119,0.05);
#4327=CYLINDRICAL_SURFACE('',#5120,0.05);
#4328=CYLINDRICAL_SURFACE('',#5121,0.05);
#4329=CYLINDRICAL_SURFACE('',#5122,0.05);
#4330=CYLINDRICAL_SURFACE('',#5123,0.05);
#4331=CYLINDRICAL_SURFACE('',#5124,0.05);
#4332=CYLINDRICAL_SURFACE('',#5125,0.0499999999999998);
#4333=CYLINDRICAL_SURFACE('',#5126,0.0499999999999998);
#4334=CYLINDRICAL_SURFACE('',#5127,0.05);
#4335=CYLINDRICAL_SURFACE('',#5128,0.05);
#4336=CYLINDRICAL_SURFACE('',#5129,0.05);
#4337=CYLINDRICAL_SURFACE('',#5130,0.05);
#4338=CYLINDRICAL_SURFACE('',#5131,0.4);
#4339=CYLINDRICAL_SURFACE('',#5135,0.6185);
#4340=CYLINDRICAL_SURFACE('',#5139,1.2);
#4341=CYLINDRICAL_SURFACE('',#5148,2.);
#4342=CYLINDRICAL_SURFACE('',#5151,0.685);
#4343=CYLINDRICAL_SURFACE('',#5154,1.9);
#4344=CYLINDRICAL_SURFACE('',#5167,0.225);
#4345=CYLINDRICAL_SURFACE('',#5170,0.225);
#4346=CYLINDRICAL_SURFACE('',#5173,0.33);
#4347=CYLINDRICAL_SURFACE('',#5176,0.33);
#4348=CYLINDRICAL_SURFACE('',#5179,0.33);
#4349=CYLINDRICAL_SURFACE('',#5182,0.33);
#4350=CYLINDRICAL_SURFACE('',#5190,3.4);
#4351=CYLINDRICAL_SURFACE('',#5209,0.685);
#4352=CYLINDRICAL_SURFACE('',#5215,0.685);
#4353=CYLINDRICAL_SURFACE('',#5221,0.46);
#4354=CYLINDRICAL_SURFACE('',#5223,0.2);
#4355=CYLINDRICAL_SURFACE('',#5226,0.6);
#4356=CYLINDRICAL_SURFACE('',#5235,0.4);
#4357=CYLINDRICAL_SURFACE('',#5243,0.4);
#4358=CYLINDRICAL_SURFACE('',#5244,0.15);
#4359=CYLINDRICAL_SURFACE('',#5246,0.15);
#4360=CYLINDRICAL_SURFACE('',#5248,0.4);
#4361=CYLINDRICAL_SURFACE('',#5254,0.16);
#4362=CYLINDRICAL_SURFACE('',#5257,2.2);
#4363=CYLINDRICAL_SURFACE('',#5263,0.275);
#4364=CYLINDRICAL_SURFACE('',#5266,0.275);
#4365=CYLINDRICAL_SURFACE('',#5269,0.275);
#4366=CYLINDRICAL_SURFACE('',#5272,0.275);
#4367=CYLINDRICAL_SURFACE('',#5275,0.275);
#4368=CYLINDRICAL_SURFACE('',#5278,0.275);
#4369=CYLINDRICAL_SURFACE('',#5281,0.16);
#4370=CYLINDRICAL_SURFACE('',#5284,4.);
#4371=CYLINDRICAL_SURFACE('',#5290,0.41);
#4372=CYLINDRICAL_SURFACE('',#5293,0.6);
#4373=CYLINDRICAL_SURFACE('',#5299,0.16);
#4374=CYLINDRICAL_SURFACE('',#5302,2.2);
#4375=CYLINDRICAL_SURFACE('',#5310,0.525);
#4376=CYLINDRICAL_SURFACE('',#5312,0.525);
#4377=CYLINDRICAL_SURFACE('',#5320,0.525);
#4378=CYLINDRICAL_SURFACE('',#5325,0.525);
#4379=CYLINDRICAL_SURFACE('',#5330,0.525);
#4380=CYLINDRICAL_SURFACE('',#5332,0.525);
#4381=CYLINDRICAL_SURFACE('',#5337,3.);
#4382=CYLINDRICAL_SURFACE('',#5346,0.275);
#4383=CYLINDRICAL_SURFACE('',#5349,0.275);
#4384=CYLINDRICAL_SURFACE('',#5352,0.275);
#4385=CYLINDRICAL_SURFACE('',#5355,0.275);
#4386=CYLINDRICAL_SURFACE('',#5358,0.275);
#4387=CYLINDRICAL_SURFACE('',#5361,0.275);
#4388=CYLINDRICAL_SURFACE('',#5364,0.34);
#4389=CYLINDRICAL_SURFACE('',#5367,2.5);
#4390=CYLINDRICAL_SURFACE('',#5372,4.);
#4391=CYLINDRICAL_SURFACE('',#5383,0.6);
#4392=CYLINDRICAL_SURFACE('',#5387,1.2);
#4393=CYLINDRICAL_SURFACE('',#5393,0.4);
#4394=CYLINDRICAL_SURFACE('',#5402,0.165);
#4395=CYLINDRICAL_SURFACE('',#5405,0.4);
#4396=CYLINDRICAL_SURFACE('',#5408,1.5);
#4397=CYLINDRICAL_SURFACE('',#5418,0.425);
#4398=CYLINDRICAL_SURFACE('',#5426,0.24505);
#4399=CYLINDRICAL_SURFACE('',#5440,0.42);
#4400=CYLINDRICAL_SURFACE('',#5443,0.8);
#4401=CYLINDRICAL_SURFACE('',#5456,0.338975);
#4402=CYLINDRICAL_SURFACE('',#5476,0.1954);
#4403=CYLINDRICAL_SURFACE('',#5486,0.225);
#4404=CYLINDRICAL_SURFACE('',#5500,0.35);
#4405=CYLINDRICAL_SURFACE('',#5508,0.1954);
#4406=ADVANCED_FACE('',(#571),#4291,.F.);
#4407=ADVANCED_FACE('',(#572),#4292,.F.);
#4408=ADVANCED_FACE('',(#573),#420,.F.);
#4409=ADVANCED_FACE('',(#574),#4293,.F.);
#4410=ADVANCED_FACE('',(#575),#421,.F.);
#4411=ADVANCED_FACE('',(#576),#4294,.F.);
#4412=ADVANCED_FACE('',(#577),#422,.F.);
#4413=ADVANCED_FACE('',(#578),#4295,.F.);
#4414=ADVANCED_FACE('',(#579),#423,.F.);
#4415=ADVANCED_FACE('',(#580),#4296,.F.);
#4416=ADVANCED_FACE('',(#581),#424,.F.);
#4417=ADVANCED_FACE('',(#582),#4297,.T.);
#4418=ADVANCED_FACE('',(#583),#4298,.F.);
#4419=ADVANCED_FACE('',(#584,#292),#425,.F.);
#4420=ADVANCED_FACE('',(#585,#293,#294,#295,#296,#297),#426,.F.);
#4421=ADVANCED_FACE('',(#586),#427,.T.);
#4422=ADVANCED_FACE('',(#587),#4299,.F.);
#4423=ADVANCED_FACE('',(#588),#4300,.F.);
#4424=ADVANCED_FACE('',(#589),#428,.T.);
#4425=ADVANCED_FACE('',(#590),#4301,.F.);
#4426=ADVANCED_FACE('',(#591),#429,.T.);
#4427=ADVANCED_FACE('',(#592),#4302,.F.);
#4428=ADVANCED_FACE('',(#593),#430,.T.);
#4429=ADVANCED_FACE('',(#594),#4303,.F.);
#4430=ADVANCED_FACE('',(#595),#431,.T.);
#4431=ADVANCED_FACE('',(#596),#4304,.F.);
#4432=ADVANCED_FACE('',(#597),#432,.T.);
#4433=ADVANCED_FACE('',(#598,#298),#433,.F.);
#4434=ADVANCED_FACE('',(#599),#434,.T.);
#4435=ADVANCED_FACE('',(#600),#435,.T.);
#4436=ADVANCED_FACE('',(#601),#4305,.F.);
#4437=ADVANCED_FACE('',(#602),#4306,.F.);
#4438=ADVANCED_FACE('',(#603),#4307,.F.);
#4439=ADVANCED_FACE('',(#604),#4308,.F.);
#4440=ADVANCED_FACE('',(#605),#4309,.F.);
#4441=ADVANCED_FACE('',(#606),#4310,.F.);
#4442=ADVANCED_FACE('',(#607),#4311,.F.);
#4443=ADVANCED_FACE('',(#608,#299),#436,.T.);
#4444=ADVANCED_FACE('',(#609),#437,.F.);
#4445=ADVANCED_FACE('',(#610),#438,.F.);
#4446=ADVANCED_FACE('',(#611),#439,.F.);
#4447=ADVANCED_FACE('',(#612),#4312,.F.);
#4448=ADVANCED_FACE('',(#613),#4313,.F.);
#4449=ADVANCED_FACE('',(#614),#4314,.F.);
#4450=ADVANCED_FACE('',(#615),#440,.F.);
#4451=ADVANCED_FACE('',(#616),#4315,.F.);
#4452=ADVANCED_FACE('',(#617,#300),#4316,.F.);
#4453=ADVANCED_FACE('',(#618,#301),#441,.F.);
#4454=ADVANCED_FACE('',(#619),#4317,.F.);
#4455=ADVANCED_FACE('',(#620,#302),#442,.F.);
#4456=ADVANCED_FACE('',(#621,#303),#443,.T.);
#4457=ADVANCED_FACE('',(#622),#4318,.F.);
#4458=ADVANCED_FACE('',(#623),#4319,.F.);
#4459=ADVANCED_FACE('',(#624),#4320,.T.);
#4460=ADVANCED_FACE('',(#625,#304),#444,.T.);
#4461=ADVANCED_FACE('',(#626,#305),#445,.F.);
#4462=ADVANCED_FACE('',(#627,#306),#4321,.F.);
#4463=ADVANCED_FACE('',(#628),#4322,.F.);
#4464=ADVANCED_FACE('',(#629,#307),#446,.F.);
#4465=ADVANCED_FACE('',(#630,#308),#4323,.F.);
#4466=ADVANCED_FACE('',(#631,#309,#310),#447,.T.);
#4467=ADVANCED_FACE('',(#632),#4324,.F.);
#4468=ADVANCED_FACE('',(#633,#311,#312),#448,.F.);
#4469=ADVANCED_FACE('',(#634,#313,#314),#4325,.T.);
#4470=ADVANCED_FACE('',(#635,#315,#316,#317,#318,#319,#320,#321),#449,.T.);
#4471=ADVANCED_FACE('',(#636,#322,#323,#324),#450,.F.);
#4472=ADVANCED_FACE('',(#637),#182,.T.);
#4473=ADVANCED_FACE('',(#638),#4326,.F.);
#4474=ADVANCED_FACE('',(#639),#4327,.F.);
#4475=ADVANCED_FACE('',(#640),#4328,.F.);
#4476=ADVANCED_FACE('',(#641),#4329,.F.);
#4477=ADVANCED_FACE('',(#642),#4330,.F.);
#4478=ADVANCED_FACE('',(#643),#4331,.F.);
#4479=ADVANCED_FACE('',(#644),#4332,.F.);
#4480=ADVANCED_FACE('',(#645),#4333,.F.);
#4481=ADVANCED_FACE('',(#646),#4334,.F.);
#4482=ADVANCED_FACE('',(#647),#4335,.F.);
#4483=ADVANCED_FACE('',(#648),#4336,.F.);
#4484=ADVANCED_FACE('',(#649),#4337,.F.);
#4485=ADVANCED_FACE('',(#650,#325,#326,#327,#328,#329,#330,#331,#332,#333),
#4338,.F.);
#4486=ADVANCED_FACE('',(#651),#451,.T.);
#4487=ADVANCED_FACE('',(#652),#4339,.T.);
#4488=ADVANCED_FACE('',(#653,#334),#452,.T.);
#4489=ADVANCED_FACE('',(#654,#335,#336,#337,#338,#339,#340,#341,#342,#343),
#4340,.T.);
#4490=ADVANCED_FACE('',(#655,#344),#453,.T.);
#4491=ADVANCED_FACE('',(#656),#454,.F.);
#4492=ADVANCED_FACE('',(#657,#345),#455,.T.);
#4493=ADVANCED_FACE('',(#658),#4341,.T.);
#4494=ADVANCED_FACE('',(#659),#456,.F.);
#4495=ADVANCED_FACE('',(#660),#4342,.T.);
#4496=ADVANCED_FACE('',(#661),#457,.T.);
#4497=ADVANCED_FACE('',(#662),#4343,.T.);
#4498=ADVANCED_FACE('',(#663),#458,.T.);
#4499=ADVANCED_FACE('',(#664),#459,.F.);
#4500=ADVANCED_FACE('',(#665),#460,.T.);
#4501=ADVANCED_FACE('',(#666),#461,.T.);
#4502=ADVANCED_FACE('',(#667),#462,.T.);
#4503=ADVANCED_FACE('',(#668),#463,.T.);
#4504=ADVANCED_FACE('',(#669),#464,.T.);
#4505=ADVANCED_FACE('',(#670),#465,.T.);
#4506=ADVANCED_FACE('',(#671),#466,.F.);
#4507=ADVANCED_FACE('',(#672),#4344,.F.);
#4508=ADVANCED_FACE('',(#673),#4345,.F.);
#4509=ADVANCED_FACE('',(#674),#4346,.F.);
#4510=ADVANCED_FACE('',(#675),#4347,.F.);
#4511=ADVANCED_FACE('',(#676),#4348,.F.);
#4512=ADVANCED_FACE('',(#677),#4349,.F.);
#4513=ADVANCED_FACE('',(#678,#346,#347),#467,.F.);
#4514=ADVANCED_FACE('',(#679,#348,#349),#468,.F.);
#4515=ADVANCED_FACE('',(#680),#469,.T.);
#4516=ADVANCED_FACE('',(#681),#470,.T.);
#4517=ADVANCED_FACE('',(#682,#350,#351,#352,#353),#471,.T.);
#4518=ADVANCED_FACE('',(#683),#4350,.F.);
#4519=ADVANCED_FACE('',(#684),#472,.T.);
#4520=ADVANCED_FACE('',(#685),#473,.T.);
#4521=ADVANCED_FACE('',(#686),#474,.T.);
#4522=ADVANCED_FACE('',(#687,#354,#355,#356),#475,.T.);
#4523=ADVANCED_FACE('',(#688,#357,#358,#359),#476,.F.);
#4524=ADVANCED_FACE('',(#689,#360),#477,.F.);
#4525=ADVANCED_FACE('',(#690,#361),#478,.T.);
#4526=ADVANCED_FACE('',(#691),#479,.T.);
#4527=ADVANCED_FACE('',(#692),#480,.T.);
#4528=ADVANCED_FACE('',(#693),#481,.T.);
#4529=ADVANCED_FACE('',(#694),#482,.T.);
#4530=ADVANCED_FACE('',(#695),#483,.T.);
#4531=ADVANCED_FACE('',(#696),#484,.T.);
#4532=ADVANCED_FACE('',(#697),#4351,.T.);
#4533=ADVANCED_FACE('',(#698,#362),#485,.T.);
#4534=ADVANCED_FACE('',(#699),#168,.T.);
#4535=ADVANCED_FACE('',(#700),#4352,.T.);
#4536=ADVANCED_FACE('',(#701),#169,.T.);
#4537=ADVANCED_FACE('',(#702,#363),#486,.T.);
#4538=ADVANCED_FACE('',(#703),#4353,.F.);
#4539=ADVANCED_FACE('',(#704),#4354,.F.);
#4540=ADVANCED_FACE('',(#705),#4355,.T.);
#4541=ADVANCED_FACE('',(#706,#364),#487,.T.);
#4542=ADVANCED_FACE('',(#707,#365),#488,.F.);
#4543=ADVANCED_FACE('',(#708,#366),#489,.F.);
#4544=ADVANCED_FACE('',(#709),#4356,.T.);
#4545=ADVANCED_FACE('',(#710,#367),#490,.T.);
#4546=ADVANCED_FACE('',(#711,#368),#491,.F.);
#4547=ADVANCED_FACE('',(#712),#4357,.T.);
#4548=ADVANCED_FACE('',(#713),#4358,.T.);
#4549=ADVANCED_FACE('',(#714),#4359,.T.);
#4550=ADVANCED_FACE('',(#715),#492,.T.);
#4551=ADVANCED_FACE('',(#716),#4360,.T.);
#4552=ADVANCED_FACE('',(#717,#369),#493,.T.);
#4553=ADVANCED_FACE('',(#718),#494,.F.);
#4554=ADVANCED_FACE('',(#719),#4361,.F.);
#4555=ADVANCED_FACE('',(#720),#4362,.T.);
#4556=ADVANCED_FACE('',(#721,#370),#495,.T.);
#4557=ADVANCED_FACE('',(#722,#371),#496,.F.);
#4558=ADVANCED_FACE('',(#723),#4363,.F.);
#4559=ADVANCED_FACE('',(#724),#4364,.F.);
#4560=ADVANCED_FACE('',(#725),#4365,.F.);
#4561=ADVANCED_FACE('',(#726),#4366,.F.);
#4562=ADVANCED_FACE('',(#727),#4367,.F.);
#4563=ADVANCED_FACE('',(#728),#4368,.F.);
#4564=ADVANCED_FACE('',(#729),#4369,.F.);
#4565=ADVANCED_FACE('',(#730),#4370,.T.);
#4566=ADVANCED_FACE('',(#731,#372,#373,#374,#375,#376,#377,#378),#497,.T.);
#4567=ADVANCED_FACE('',(#732,#379,#380,#381,#382,#383,#384,#385),#498,.F.);
#4568=ADVANCED_FACE('',(#733),#4371,.F.);
#4569=ADVANCED_FACE('',(#734),#4372,.T.);
#4570=ADVANCED_FACE('',(#735,#386),#499,.T.);
#4571=ADVANCED_FACE('',(#736,#387),#500,.T.);
#4572=ADVANCED_FACE('',(#737),#4373,.F.);
#4573=ADVANCED_FACE('',(#738),#4374,.T.);
#4574=ADVANCED_FACE('',(#739,#388),#501,.T.);
#4575=ADVANCED_FACE('',(#740,#389),#502,.F.);
#4576=ADVANCED_FACE('',(#741),#503,.F.);
#4577=ADVANCED_FACE('',(#742),#4375,.F.);
#4578=ADVANCED_FACE('',(#743),#4376,.F.);
#4579=ADVANCED_FACE('',(#744),#504,.F.);
#4580=ADVANCED_FACE('',(#745),#505,.F.);
#4581=ADVANCED_FACE('',(#746),#4377,.F.);
#4582=ADVANCED_FACE('',(#747),#506,.F.);
#4583=ADVANCED_FACE('',(#748),#4378,.F.);
#4584=ADVANCED_FACE('',(#749),#507,.F.);
#4585=ADVANCED_FACE('',(#750),#4379,.F.);
#4586=ADVANCED_FACE('',(#751),#4380,.F.);
#4587=ADVANCED_FACE('',(#752),#508,.F.);
#4588=ADVANCED_FACE('',(#753),#4381,.T.);
#4589=ADVANCED_FACE('',(#754),#4382,.F.);
#4590=ADVANCED_FACE('',(#755),#4383,.F.);
#4591=ADVANCED_FACE('',(#756),#4384,.F.);
#4592=ADVANCED_FACE('',(#757),#4385,.F.);
#4593=ADVANCED_FACE('',(#758),#4386,.F.);
#4594=ADVANCED_FACE('',(#759),#4387,.F.);
#4595=ADVANCED_FACE('',(#760),#4388,.F.);
#4596=ADVANCED_FACE('',(#761),#4389,.F.);
#4597=ADVANCED_FACE('',(#762,#390),#509,.F.);
#4598=ADVANCED_FACE('',(#763,#391),#510,.T.);
#4599=ADVANCED_FACE('',(#764),#4390,.T.);
#4600=ADVANCED_FACE('',(#765,#392,#393,#394,#395,#396,#397,#398),#511,.T.);
#4601=ADVANCED_FACE('',(#766,#399,#400,#401,#402,#403,#404,#405),#512,.F.);
#4602=ADVANCED_FACE('',(#767),#167,.T.);
#4603=ADVANCED_FACE('',(#768),#513,.T.);
#4604=ADVANCED_FACE('',(#769),#514,.F.);
#4605=ADVANCED_FACE('',(#770),#4391,.T.);
#4606=ADVANCED_FACE('',(#771),#515,.F.);
#4607=ADVANCED_FACE('',(#772),#4392,.T.);
#4608=ADVANCED_FACE('',(#773),#516,.T.);
#4609=ADVANCED_FACE('',(#774,#406),#517,.F.);
#4610=ADVANCED_FACE('',(#775),#4393,.T.);
#4611=ADVANCED_FACE('',(#776),#518,.T.);
#4612=ADVANCED_FACE('',(#777),#519,.F.);
#4613=ADVANCED_FACE('',(#778),#520,.T.);
#4614=ADVANCED_FACE('',(#779),#4394,.F.);
#4615=ADVANCED_FACE('',(#780),#521,.T.);
#4616=ADVANCED_FACE('',(#781,#407),#4395,.F.);
#4617=ADVANCED_FACE('',(#782,#408),#4396,.T.);
#4618=ADVANCED_FACE('',(#783,#409),#522,.T.);
#4619=ADVANCED_FACE('',(#784,#410),#523,.F.);
#4620=ADVANCED_FACE('',(#785),#524,.T.);
#4621=ADVANCED_FACE('',(#786),#170,.T.);
#4622=ADVANCED_FACE('',(#787),#4397,.T.);
#4623=ADVANCED_FACE('',(#788),#171,.T.);
#4624=ADVANCED_FACE('',(#789,#411),#525,.T.);
#4625=ADVANCED_FACE('',(#790),#172,.T.);
#4626=ADVANCED_FACE('',(#791),#4398,.T.);
#4627=ADVANCED_FACE('',(#792),#173,.T.);
#4628=ADVANCED_FACE('',(#793),#526,.T.);
#4629=ADVANCED_FACE('',(#794),#527,.F.);
#4630=ADVANCED_FACE('',(#795),#528,.F.);
#4631=ADVANCED_FACE('',(#796),#529,.F.);
#4632=ADVANCED_FACE('',(#797),#530,.F.);
#4633=ADVANCED_FACE('',(#798),#531,.F.);
#4634=ADVANCED_FACE('',(#799),#532,.F.);
#4635=ADVANCED_FACE('',(#800),#533,.F.);
#4636=ADVANCED_FACE('',(#801),#534,.F.);
#4637=ADVANCED_FACE('',(#802),#4399,.F.);
#4638=ADVANCED_FACE('',(#803),#4400,.T.);
#4639=ADVANCED_FACE('',(#804,#412),#535,.T.);
#4640=ADVANCED_FACE('',(#805,#413),#536,.F.);
#4641=ADVANCED_FACE('',(#806),#174,.T.);
#4642=ADVANCED_FACE('',(#807),#175,.T.);
#4643=ADVANCED_FACE('',(#808),#537,.T.);
#4644=ADVANCED_FACE('',(#809),#538,.T.);
#4645=ADVANCED_FACE('',(#810),#539,.T.);
#4646=ADVANCED_FACE('',(#811),#4401,.F.);
#4647=ADVANCED_FACE('',(#812),#540,.T.);
#4648=ADVANCED_FACE('',(#813),#541,.T.);
#4649=ADVANCED_FACE('',(#814),#542,.T.);
#4650=ADVANCED_FACE('',(#815,#414),#543,.T.);
#4651=ADVANCED_FACE('',(#816,#415),#544,.F.);
#4652=ADVANCED_FACE('',(#817),#545,.F.);
#4653=ADVANCED_FACE('',(#818),#546,.F.);
#4654=ADVANCED_FACE('',(#819),#547,.F.);
#4655=ADVANCED_FACE('',(#820),#548,.F.);
#4656=ADVANCED_FACE('',(#821),#549,.F.);
#4657=ADVANCED_FACE('',(#822),#550,.F.);
#4658=ADVANCED_FACE('',(#823),#551,.F.);
#4659=ADVANCED_FACE('',(#824,#416),#552,.T.);
#4660=ADVANCED_FACE('',(#825),#176,.T.);
#4661=ADVANCED_FACE('',(#826),#4402,.T.);
#4662=ADVANCED_FACE('',(#827),#177,.T.);
#4663=ADVANCED_FACE('',(#828),#553,.T.);
#4664=ADVANCED_FACE('',(#829),#183,.T.);
#4665=ADVANCED_FACE('',(#830),#4403,.F.);
#4666=ADVANCED_FACE('',(#831),#554,.T.);
#4667=ADVANCED_FACE('',(#832),#555,.T.);
#4668=ADVANCED_FACE('',(#833),#556,.T.);
#4669=ADVANCED_FACE('',(#834),#557,.T.);
#4670=ADVANCED_FACE('',(#835,#417),#558,.T.);
#4671=ADVANCED_FACE('',(#836,#418),#559,.F.);
#4672=ADVANCED_FACE('',(#837),#560,.T.);
#4673=ADVANCED_FACE('',(#838),#178,.T.);
#4674=ADVANCED_FACE('',(#839),#4404,.T.);
#4675=ADVANCED_FACE('',(#840),#179,.T.);
#4676=ADVANCED_FACE('',(#841,#419),#561,.T.);
#4677=ADVANCED_FACE('',(#842),#180,.T.);
#4678=ADVANCED_FACE('',(#843),#4405,.T.);
#4679=ADVANCED_FACE('',(#844),#181,.T.);
#4680=ADVANCED_FACE('',(#845),#562,.T.);
#4681=ADVANCED_FACE('',(#846),#563,.F.);
#4682=ADVANCED_FACE('',(#847),#564,.F.);
#4683=ADVANCED_FACE('',(#848),#565,.F.);
#4684=ADVANCED_FACE('',(#849),#566,.F.);
#4685=ADVANCED_FACE('',(#850),#567,.F.);
#4686=ADVANCED_FACE('',(#851),#568,.F.);
#4687=ADVANCED_FACE('',(#852),#569,.F.);
#4688=ADVANCED_FACE('',(#853),#570,.F.);
#4689=CLOSED_SHELL('',(#4406,#4407,#4408,#4409,#4410,#4411,#4412,#4413,
#4414,#4415,#4416,#4417,#4418,#4419,#4420,#4421,#4422,#4423,#4424,#4425,
#4426,#4427,#4428,#4429,#4430,#4431,#4432,#4433,#4434,#4435,#4436,#4437,
#4438,#4439,#4440,#4441,#4442,#4443,#4444,#4445,#4446,#4447,#4448,#4449,
#4450,#4451,#4452,#4453,#4454,#4455,#4456,#4457,#4458,#4459,#4460,#4461,
#4462,#4463,#4464,#4465,#4466,#4467,#4468,#4469,#4470,#4471));
#4690=CLOSED_SHELL('',(#4472));
#4691=CLOSED_SHELL('',(#4473,#4474,#4475,#4476,#4477,#4478,#4479,#4480,
#4481,#4482,#4483,#4484,#4485,#4486,#4487,#4488,#4489,#4490,#4491));
#4692=CLOSED_SHELL('',(#4492,#4493,#4494,#4495,#4496));
#4693=CLOSED_SHELL('',(#4497,#4498,#4499));
#4694=CLOSED_SHELL('',(#4500,#4501,#4502,#4503,#4504,#4505,#4506));
#4695=CLOSED_SHELL('',(#4507,#4508,#4509,#4510,#4511,#4512,#4513,#4514,
#4515,#4516,#4517,#4518,#4519,#4520,#4521,#4522,#4523));
#4696=CLOSED_SHELL('',(#4524,#4525,#4526,#4527,#4528,#4529,#4530,#4531,
#4532,#4533,#4534,#4535,#4536,#4537,#4538));
#4697=CLOSED_SHELL('',(#4539,#4540,#4541,#4542));
#4698=CLOSED_SHELL('',(#4543,#4544,#4545,#4546,#4547,#4548,#4549,#4550,
#4551,#4552,#4553));
#4699=CLOSED_SHELL('',(#4554,#4555,#4556,#4557));
#4700=CLOSED_SHELL('',(#4558,#4559,#4560,#4561,#4562,#4563,#4564,#4565,
#4566,#4567));
#4701=CLOSED_SHELL('',(#4568,#4569,#4570,#4571,#4572,#4573,#4574,#4575));
#4702=CLOSED_SHELL('',(#4576,#4577,#4578,#4579,#4580,#4581,#4582,#4583,
#4584,#4585,#4586,#4587,#4588,#4589,#4590,#4591,#4592,#4593,#4594,#4595,
#4596,#4597,#4598,#4599,#4600,#4601));
#4703=CLOSED_SHELL('',(#4602,#4603,#4604));
#4704=CLOSED_SHELL('',(#4605,#4606,#4607,#4608,#4609));
#4705=CLOSED_SHELL('',(#4610,#4611,#4612));
#4706=CLOSED_SHELL('',(#4613,#4614,#4615,#4616,#4617,#4618,#4619));
#4707=CLOSED_SHELL('',(#4620,#4621,#4622,#4623,#4624,#4625,#4626,#4627,
#4628));
#4708=CLOSED_SHELL('',(#4629,#4630,#4631,#4632,#4633,#4634,#4635,#4636));
#4709=CLOSED_SHELL('',(#4637,#4638,#4639,#4640));
#4710=CLOSED_SHELL('',(#4641,#4642,#4643,#4644,#4645,#4646,#4647,#4648,
#4649,#4650,#4651));
#4711=CLOSED_SHELL('',(#4652,#4653,#4654,#4655,#4656,#4657,#4658,#4659,
#4660,#4661,#4662,#4663));
#4712=CLOSED_SHELL('',(#4664));
#4713=CLOSED_SHELL('',(#4665,#4666,#4667,#4668,#4669,#4670,#4671));
#4714=CLOSED_SHELL('',(#4672,#4673,#4674,#4675,#4676,#4677,#4678,#4679,
#4680));
#4715=CLOSED_SHELL('',(#4681,#4682,#4683,#4684,#4685,#4686,#4687,#4688));
#4716=DERIVED_UNIT_ELEMENT(#4762,1.);
#4717=DERIVED_UNIT_ELEMENT(#10268,-3.);
#4718=DERIVED_UNIT_ELEMENT(#4762,1.);
#4719=DERIVED_UNIT_ELEMENT(#10268,-3.);
#4720=DERIVED_UNIT_ELEMENT(#4762,1.);
#4721=DERIVED_UNIT_ELEMENT(#10268,-3.);
#4722=DERIVED_UNIT_ELEMENT(#4762,1.);
#4723=DERIVED_UNIT_ELEMENT(#10268,-3.);
#4724=DERIVED_UNIT_ELEMENT(#4762,1.);
#4725=DERIVED_UNIT_ELEMENT(#10268,-3.);
#4726=DERIVED_UNIT_ELEMENT(#4762,1.);
#4727=DERIVED_UNIT_ELEMENT(#10268,-3.);
#4728=DERIVED_UNIT_ELEMENT(#4762,1.);
#4729=DERIVED_UNIT_ELEMENT(#10268,-3.);
#4730=DERIVED_UNIT_ELEMENT(#4762,1.);
#4731=DERIVED_UNIT_ELEMENT(#10268,-3.);
#4732=DERIVED_UNIT_ELEMENT(#4762,1.);
#4733=DERIVED_UNIT_ELEMENT(#10268,-3.);
#4734=DERIVED_UNIT_ELEMENT(#4762,1.);
#4735=DERIVED_UNIT_ELEMENT(#10268,-3.);
#4736=DERIVED_UNIT_ELEMENT(#4762,1.);
#4737=DERIVED_UNIT_ELEMENT(#10268,-3.);
#4738=DERIVED_UNIT_ELEMENT(#4762,1.);
#4739=DERIVED_UNIT_ELEMENT(#10268,-3.);
#4740=DERIVED_UNIT_ELEMENT(#4762,1.);
#4741=DERIVED_UNIT_ELEMENT(#10268,-3.);
#4742=DERIVED_UNIT_ELEMENT(#4762,1.);
#4743=DERIVED_UNIT_ELEMENT(#10268,-3.);
#4744=DERIVED_UNIT_ELEMENT(#4762,1.);
#4745=DERIVED_UNIT_ELEMENT(#10268,-3.);
#4746=DERIVED_UNIT_ELEMENT(#4762,1.);
#4747=DERIVED_UNIT_ELEMENT(#10268,-3.);
#4748=DERIVED_UNIT_ELEMENT(#4762,1.);
#4749=DERIVED_UNIT_ELEMENT(#10268,-3.);
#4750=DERIVED_UNIT_ELEMENT(#4762,1.);
#4751=DERIVED_UNIT_ELEMENT(#10268,-3.);
#4752=DERIVED_UNIT_ELEMENT(#4762,1.);
#4753=DERIVED_UNIT_ELEMENT(#10268,-3.);
#4754=DERIVED_UNIT_ELEMENT(#4762,1.);
#4755=DERIVED_UNIT_ELEMENT(#10268,-3.);
#4756=DERIVED_UNIT_ELEMENT(#4762,1.);
#4757=DERIVED_UNIT_ELEMENT(#10268,-3.);
#4758=DERIVED_UNIT_ELEMENT(#4762,1.);
#4759=DERIVED_UNIT_ELEMENT(#10268,-3.);
#4760=DERIVED_UNIT_ELEMENT(#4762,1.);
#4761=DERIVED_UNIT_ELEMENT(#10268,-3.);
#4762=(
MASS_UNIT()
NAMED_UNIT(*)
SI_UNIT(.KILO.,.GRAM.)
);
#4763=DERIVED_UNIT((#4716,#4717));
#4764=DERIVED_UNIT((#4718,#4719));
#4765=DERIVED_UNIT((#4720,#4721));
#4766=DERIVED_UNIT((#4722,#4723));
#4767=DERIVED_UNIT((#4724,#4725));
#4768=DERIVED_UNIT((#4726,#4727));
#4769=DERIVED_UNIT((#4728,#4729));
#4770=DERIVED_UNIT((#4730,#4731));
#4771=DERIVED_UNIT((#4732,#4733));
#4772=DERIVED_UNIT((#4734,#4735));
#4773=DERIVED_UNIT((#4736,#4737));
#4774=DERIVED_UNIT((#4738,#4739));
#4775=DERIVED_UNIT((#4740,#4741));
#4776=DERIVED_UNIT((#4742,#4743));
#4777=DERIVED_UNIT((#4744,#4745));
#4778=DERIVED_UNIT((#4746,#4747));
#4779=DERIVED_UNIT((#4748,#4749));
#4780=DERIVED_UNIT((#4750,#4751));
#4781=DERIVED_UNIT((#4752,#4753));
#4782=DERIVED_UNIT((#4754,#4755));
#4783=DERIVED_UNIT((#4756,#4757));
#4784=DERIVED_UNIT((#4758,#4759));
#4785=DERIVED_UNIT((#4760,#4761));
#4786=MEASURE_REPRESENTATION_ITEM('density measure',
POSITIVE_RATIO_MEASURE(7850.),#4763);
#4787=MEASURE_REPRESENTATION_ITEM('density measure',
POSITIVE_RATIO_MEASURE(7850.),#4764);
#4788=MEASURE_REPRESENTATION_ITEM('density measure',
POSITIVE_RATIO_MEASURE(7850.),#4765);
#4789=MEASURE_REPRESENTATION_ITEM('density measure',
POSITIVE_RATIO_MEASURE(7850.),#4766);
#4790=MEASURE_REPRESENTATION_ITEM('density measure',
POSITIVE_RATIO_MEASURE(7850.),#4767);
#4791=MEASURE_REPRESENTATION_ITEM('density measure',
POSITIVE_RATIO_MEASURE(7850.),#4768);
#4792=MEASURE_REPRESENTATION_ITEM('density measure',
POSITIVE_RATIO_MEASURE(7850.),#4769);
#4793=MEASURE_REPRESENTATION_ITEM('density measure',
POSITIVE_RATIO_MEASURE(7850.),#4770);
#4794=MEASURE_REPRESENTATION_ITEM('density measure',
POSITIVE_RATIO_MEASURE(7850.),#4771);
#4795=MEASURE_REPRESENTATION_ITEM('density measure',
POSITIVE_RATIO_MEASURE(7850.),#4772);
#4796=MEASURE_REPRESENTATION_ITEM('density measure',
POSITIVE_RATIO_MEASURE(7850.),#4773);
#4797=MEASURE_REPRESENTATION_ITEM('density measure',
POSITIVE_RATIO_MEASURE(7850.),#4774);
#4798=MEASURE_REPRESENTATION_ITEM('density measure',
POSITIVE_RATIO_MEASURE(7850.),#4775);
#4799=MEASURE_REPRESENTATION_ITEM('density measure',
POSITIVE_RATIO_MEASURE(7850.),#4776);
#4800=MEASURE_REPRESENTATION_ITEM('density measure',
POSITIVE_RATIO_MEASURE(7850.),#4777);
#4801=MEASURE_REPRESENTATION_ITEM('density measure',
POSITIVE_RATIO_MEASURE(7850.),#4778);
#4802=MEASURE_REPRESENTATION_ITEM('density measure',
POSITIVE_RATIO_MEASURE(7850.),#4779);
#4803=MEASURE_REPRESENTATION_ITEM('density measure',
POSITIVE_RATIO_MEASURE(7850.),#4780);
#4804=MEASURE_REPRESENTATION_ITEM('density measure',
POSITIVE_RATIO_MEASURE(7850.),#4781);
#4805=MEASURE_REPRESENTATION_ITEM('density measure',
POSITIVE_RATIO_MEASURE(7850.),#4782);
#4806=MEASURE_REPRESENTATION_ITEM('density measure',
POSITIVE_RATIO_MEASURE(7850.),#4783);
#4807=MEASURE_REPRESENTATION_ITEM('density measure',
POSITIVE_RATIO_MEASURE(7850.),#4784);
#4808=MEASURE_REPRESENTATION_ITEM('density measure',
POSITIVE_RATIO_MEASURE(7850.),#4785);
#4809=PROPERTY_DEFINITION_REPRESENTATION(#4924,#4855);
#4810=PROPERTY_DEFINITION_REPRESENTATION(#4925,#4856);
#4811=PROPERTY_DEFINITION_REPRESENTATION(#4926,#4857);
#4812=PROPERTY_DEFINITION_REPRESENTATION(#4927,#4858);
#4813=PROPERTY_DEFINITION_REPRESENTATION(#4928,#4859);
#4814=PROPERTY_DEFINITION_REPRESENTATION(#4929,#4860);
#4815=PROPERTY_DEFINITION_REPRESENTATION(#4930,#4861);
#4816=PROPERTY_DEFINITION_REPRESENTATION(#4931,#4862);
#4817=PROPERTY_DEFINITION_REPRESENTATION(#4932,#4863);
#4818=PROPERTY_DEFINITION_REPRESENTATION(#4933,#4864);
#4819=PROPERTY_DEFINITION_REPRESENTATION(#4934,#4865);
#4820=PROPERTY_DEFINITION_REPRESENTATION(#4935,#4866);
#4821=PROPERTY_DEFINITION_REPRESENTATION(#4936,#4867);
#4822=PROPERTY_DEFINITION_REPRESENTATION(#4937,#4868);
#4823=PROPERTY_DEFINITION_REPRESENTATION(#4938,#4869);
#4824=PROPERTY_DEFINITION_REPRESENTATION(#4939,#4870);
#4825=PROPERTY_DEFINITION_REPRESENTATION(#4940,#4871);
#4826=PROPERTY_DEFINITION_REPRESENTATION(#4941,#4872);
#4827=PROPERTY_DEFINITION_REPRESENTATION(#4942,#4873);
#4828=PROPERTY_DEFINITION_REPRESENTATION(#4943,#4874);
#4829=PROPERTY_DEFINITION_REPRESENTATION(#4944,#4875);
#4830=PROPERTY_DEFINITION_REPRESENTATION(#4945,#4876);
#4831=PROPERTY_DEFINITION_REPRESENTATION(#4946,#4877);
#4832=PROPERTY_DEFINITION_REPRESENTATION(#4947,#4878);
#4833=PROPERTY_DEFINITION_REPRESENTATION(#4948,#4879);
#4834=PROPERTY_DEFINITION_REPRESENTATION(#4949,#4880);
#4835=PROPERTY_DEFINITION_REPRESENTATION(#4950,#4881);
#4836=PROPERTY_DEFINITION_REPRESENTATION(#4951,#4882);
#4837=PROPERTY_DEFINITION_REPRESENTATION(#4952,#4883);
#4838=PROPERTY_DEFINITION_REPRESENTATION(#4953,#4884);
#4839=PROPERTY_DEFINITION_REPRESENTATION(#4954,#4885);
#4840=PROPERTY_DEFINITION_REPRESENTATION(#4955,#4886);
#4841=PROPERTY_DEFINITION_REPRESENTATION(#4956,#4887);
#4842=PROPERTY_DEFINITION_REPRESENTATION(#4957,#4888);
#4843=PROPERTY_DEFINITION_REPRESENTATION(#4958,#4889);
#4844=PROPERTY_DEFINITION_REPRESENTATION(#4959,#4890);
#4845=PROPERTY_DEFINITION_REPRESENTATION(#4960,#4891);
#4846=PROPERTY_DEFINITION_REPRESENTATION(#4961,#4892);
#4847=PROPERTY_DEFINITION_REPRESENTATION(#4962,#4893);
#4848=PROPERTY_DEFINITION_REPRESENTATION(#4963,#4894);
#4849=PROPERTY_DEFINITION_REPRESENTATION(#4964,#4895);
#4850=PROPERTY_DEFINITION_REPRESENTATION(#4965,#4896);
#4851=PROPERTY_DEFINITION_REPRESENTATION(#4966,#4897);
#4852=PROPERTY_DEFINITION_REPRESENTATION(#4967,#4898);
#4853=PROPERTY_DEFINITION_REPRESENTATION(#4968,#4899);
#4854=PROPERTY_DEFINITION_REPRESENTATION(#4969,#4900);
#4855=REPRESENTATION('material name',(#4901),#10243);
#4856=REPRESENTATION('density',(#4786),#10243);
#4857=REPRESENTATION('material name',(#4902),#10244);
#4858=REPRESENTATION('density',(#4787),#10244);
#4859=REPRESENTATION('material name',(#4903),#10245);
#4860=REPRESENTATION('density',(#4788),#10245);
#4861=REPRESENTATION('material name',(#4904),#10246);
#4862=REPRESENTATION('density',(#4789),#10246);
#4863=REPRESENTATION('material name',(#4905),#10247);
#4864=REPRESENTATION('density',(#4790),#10247);
#4865=REPRESENTATION('material name',(#4906),#10248);
#4866=REPRESENTATION('density',(#4791),#10248);
#4867=REPRESENTATION('material name',(#4907),#10249);
#4868=REPRESENTATION('density',(#4792),#10249);
#4869=REPRESENTATION('material name',(#4908),#10250);
#4870=REPRESENTATION('density',(#4793),#10250);
#4871=REPRESENTATION('material name',(#4909),#10251);
#4872=REPRESENTATION('density',(#4794),#10251);
#4873=REPRESENTATION('material name',(#4910),#10252);
#4874=REPRESENTATION('density',(#4795),#10252);
#4875=REPRESENTATION('material name',(#4911),#10253);
#4876=REPRESENTATION('density',(#4796),#10253);
#4877=REPRESENTATION('material name',(#4912),#10254);
#4878=REPRESENTATION('density',(#4797),#10254);
#4879=REPRESENTATION('material name',(#4913),#10255);
#4880=REPRESENTATION('density',(#4798),#10255);
#4881=REPRESENTATION('material name',(#4914),#10256);
#4882=REPRESENTATION('density',(#4799),#10256);
#4883=REPRESENTATION('material name',(#4915),#10257);
#4884=REPRESENTATION('density',(#4800),#10257);
#4885=REPRESENTATION('material name',(#4916),#10258);
#4886=REPRESENTATION('density',(#4801),#10258);
#4887=REPRESENTATION('material name',(#4917),#10259);
#4888=REPRESENTATION('density',(#4802),#10259);
#4889=REPRESENTATION('material name',(#4918),#10260);
#4890=REPRESENTATION('density',(#4803),#10260);
#4891=REPRESENTATION('material name',(#4919),#10261);
#4892=REPRESENTATION('density',(#4804),#10261);
#4893=REPRESENTATION('material name',(#4920),#10262);
#4894=REPRESENTATION('density',(#4805),#10262);
#4895=REPRESENTATION('material name',(#4921),#10263);
#4896=REPRESENTATION('density',(#4806),#10263);
#4897=REPRESENTATION('material name',(#4922),#10264);
#4898=REPRESENTATION('density',(#4807),#10264);
#4899=REPRESENTATION('material name',(#4923),#10265);
#4900=REPRESENTATION('density',(#4808),#10265);
#4901=DESCRIPTIVE_REPRESENTATION_ITEM('Steel','Steel');
#4902=DESCRIPTIVE_REPRESENTATION_ITEM('Steel','Steel');
#4903=DESCRIPTIVE_REPRESENTATION_ITEM('Steel','Steel');
#4904=DESCRIPTIVE_REPRESENTATION_ITEM('Steel','Steel');
#4905=DESCRIPTIVE_REPRESENTATION_ITEM('Steel','Steel');
#4906=DESCRIPTIVE_REPRESENTATION_ITEM('Steel','Steel');
#4907=DESCRIPTIVE_REPRESENTATION_ITEM('Steel','Steel');
#4908=DESCRIPTIVE_REPRESENTATION_ITEM('Steel','Steel');
#4909=DESCRIPTIVE_REPRESENTATION_ITEM('Steel','Steel');
#4910=DESCRIPTIVE_REPRESENTATION_ITEM('Steel','Steel');
#4911=DESCRIPTIVE_REPRESENTATION_ITEM('Steel','Steel');
#4912=DESCRIPTIVE_REPRESENTATION_ITEM('Steel','Steel');
#4913=DESCRIPTIVE_REPRESENTATION_ITEM('Steel','Steel');
#4914=DESCRIPTIVE_REPRESENTATION_ITEM('Steel','Steel');
#4915=DESCRIPTIVE_REPRESENTATION_ITEM('Steel','Steel');
#4916=DESCRIPTIVE_REPRESENTATION_ITEM('Steel','Steel');
#4917=DESCRIPTIVE_REPRESENTATION_ITEM('Steel','Steel');
#4918=DESCRIPTIVE_REPRESENTATION_ITEM('Steel','Steel');
#4919=DESCRIPTIVE_REPRESENTATION_ITEM('Steel','Steel');
#4920=DESCRIPTIVE_REPRESENTATION_ITEM('Steel','Steel');
#4921=DESCRIPTIVE_REPRESENTATION_ITEM('Steel','Steel');
#4922=DESCRIPTIVE_REPRESENTATION_ITEM('Steel','Steel');
#4923=DESCRIPTIVE_REPRESENTATION_ITEM('Steel','Steel');
#4924=PROPERTY_DEFINITION('material property','material name',#10380);
#4925=PROPERTY_DEFINITION('material property','density of part',#10380);
#4926=PROPERTY_DEFINITION('material property','material name',#10381);
#4927=PROPERTY_DEFINITION('material property','density of part',#10381);
#4928=PROPERTY_DEFINITION('material property','material name',#10382);
#4929=PROPERTY_DEFINITION('material property','density of part',#10382);
#4930=PROPERTY_DEFINITION('material property','material name',#10383);
#4931=PROPERTY_DEFINITION('material property','density of part',#10383);
#4932=PROPERTY_DEFINITION('material property','material name',#10384);
#4933=PROPERTY_DEFINITION('material property','density of part',#10384);
#4934=PROPERTY_DEFINITION('material property','material name',#10385);
#4935=PROPERTY_DEFINITION('material property','density of part',#10385);
#4936=PROPERTY_DEFINITION('material property','material name',#10386);
#4937=PROPERTY_DEFINITION('material property','density of part',#10386);
#4938=PROPERTY_DEFINITION('material property','material name',#10387);
#4939=PROPERTY_DEFINITION('material property','density of part',#10387);
#4940=PROPERTY_DEFINITION('material property','material name',#10388);
#4941=PROPERTY_DEFINITION('material property','density of part',#10388);
#4942=PROPERTY_DEFINITION('material property','material name',#10389);
#4943=PROPERTY_DEFINITION('material property','density of part',#10389);
#4944=PROPERTY_DEFINITION('material property','material name',#10390);
#4945=PROPERTY_DEFINITION('material property','density of part',#10390);
#4946=PROPERTY_DEFINITION('material property','material name',#10391);
#4947=PROPERTY_DEFINITION('material property','density of part',#10391);
#4948=PROPERTY_DEFINITION('material property','material name',#10392);
#4949=PROPERTY_DEFINITION('material property','density of part',#10392);
#4950=PROPERTY_DEFINITION('material property','material name',#10393);
#4951=PROPERTY_DEFINITION('material property','density of part',#10393);
#4952=PROPERTY_DEFINITION('material property','material name',#10394);
#4953=PROPERTY_DEFINITION('material property','density of part',#10394);
#4954=PROPERTY_DEFINITION('material property','material name',#10395);
#4955=PROPERTY_DEFINITION('material property','density of part',#10395);
#4956=PROPERTY_DEFINITION('material property','material name',#10396);
#4957=PROPERTY_DEFINITION('material property','density of part',#10396);
#4958=PROPERTY_DEFINITION('material property','material name',#10397);
#4959=PROPERTY_DEFINITION('material property','density of part',#10397);
#4960=PROPERTY_DEFINITION('material property','material name',#10398);
#4961=PROPERTY_DEFINITION('material property','density of part',#10398);
#4962=PROPERTY_DEFINITION('material property','material name',#10399);
#4963=PROPERTY_DEFINITION('material property','density of part',#10399);
#4964=PROPERTY_DEFINITION('material property','material name',#10400);
#4965=PROPERTY_DEFINITION('material property','density of part',#10400);
#4966=PROPERTY_DEFINITION('material property','material name',#10401);
#4967=PROPERTY_DEFINITION('material property','density of part',#10401);
#4968=PROPERTY_DEFINITION('material property','material name',#10402);
#4969=PROPERTY_DEFINITION('material property','density of part',#10402);
#4970=AXIS2_PLACEMENT_3D('',#7008,#5556,#5557);
#4971=AXIS2_PLACEMENT_3D('',#7009,#5558,#5559);
#4972=AXIS2_PLACEMENT_3D('',#7010,#5560,#5561);
#4973=AXIS2_PLACEMENT_3D('',#7012,#5562,#5563);
#4974=AXIS2_PLACEMENT_3D('',#7052,#5565,#5566);
#4975=AXIS2_PLACEMENT_3D('',#7054,#5567,#5568);
#4976=AXIS2_PLACEMENT_3D('',#7057,#5570,#5571);
#4977=AXIS2_PLACEMENT_3D('',#7058,#5572,#5573);
#4978=AXIS2_PLACEMENT_3D('',#7059,#5574,#5575);
#4979=AXIS2_PLACEMENT_3D('',#7061,#5576,#5577);
#4980=AXIS2_PLACEMENT_3D('',#7064,#5579,#5580);
#4981=AXIS2_PLACEMENT_3D('',#7065,#5581,#5582);
#4982=AXIS2_PLACEMENT_3D('',#7066,#5583,#5584);
#4983=AXIS2_PLACEMENT_3D('',#7068,#5585,#5586);
#4984=AXIS2_PLACEMENT_3D('',#7071,#5588,#5589);
#4985=AXIS2_PLACEMENT_3D('',#7072,#5590,#5591);
#4986=AXIS2_PLACEMENT_3D('',#7073,#5592,#5593);
#4987=AXIS2_PLACEMENT_3D('',#7075,#5594,#5595);
#4988=AXIS2_PLACEMENT_3D('',#7078,#5597,#5598);
#4989=AXIS2_PLACEMENT_3D('',#7079,#5599,#5600);
#4990=AXIS2_PLACEMENT_3D('',#7080,#5601,#5602);
#4991=AXIS2_PLACEMENT_3D('',#7082,#5603,#5604);
#4992=AXIS2_PLACEMENT_3D('',#7085,#5606,#5607);
#4993=AXIS2_PLACEMENT_3D('',#7086,#5608,#5609);
#4994=AXIS2_PLACEMENT_3D('',#7087,#5610,#5611);
#4995=AXIS2_PLACEMENT_3D('',#7089,#5612,#5613);
#4996=AXIS2_PLACEMENT_3D('',#7092,#5615,#5616);
#4997=AXIS2_PLACEMENT_3D('',#7093,#5617,#5618);
#4998=AXIS2_PLACEMENT_3D('',#7095,#5619,#5620);
#4999=AXIS2_PLACEMENT_3D('',#7098,#5622,#5623);
#5000=AXIS2_PLACEMENT_3D('',#7099,#5624,#5625);
#5001=AXIS2_PLACEMENT_3D('',#7100,#5626,#5627);
#5002=AXIS2_PLACEMENT_3D('',#7102,#5628,#5629);
#5003=AXIS2_PLACEMENT_3D('',#7103,#5630,#5631);
#5004=AXIS2_PLACEMENT_3D('',#7108,#5633,#5634);
#5005=AXIS2_PLACEMENT_3D('',#7109,#5635,#5636);
#5006=AXIS2_PLACEMENT_3D('',#7110,#5637,#5638);
#5007=AXIS2_PLACEMENT_3D('',#7131,#5642,#5643);
#5008=AXIS2_PLACEMENT_3D('',#7132,#5644,#5645);
#5009=AXIS2_PLACEMENT_3D('',#7134,#5646,#5647);
#5010=AXIS2_PLACEMENT_3D('',#7137,#5649,#5650);
#5011=AXIS2_PLACEMENT_3D('',#7138,#5651,#5652);
#5012=AXIS2_PLACEMENT_3D('',#7139,#5653,#5654);
#5013=AXIS2_PLACEMENT_3D('',#7141,#5655,#5656);
#5014=AXIS2_PLACEMENT_3D('',#7144,#5658,#5659);
#5015=AXIS2_PLACEMENT_3D('',#7145,#5660,#5661);
#5016=AXIS2_PLACEMENT_3D('',#7146,#5662,#5663);
#5017=AXIS2_PLACEMENT_3D('',#7148,#5664,#5665);
#5018=AXIS2_PLACEMENT_3D('',#7151,#5667,#5668);
#5019=AXIS2_PLACEMENT_3D('',#7152,#5669,#5670);
#5020=AXIS2_PLACEMENT_3D('',#7153,#5671,#5672);
#5021=AXIS2_PLACEMENT_3D('',#7155,#5673,#5674);
#5022=AXIS2_PLACEMENT_3D('',#7158,#5676,#5677);
#5023=AXIS2_PLACEMENT_3D('',#7159,#5678,#5679);
#5024=AXIS2_PLACEMENT_3D('',#7160,#5680,#5681);
#5025=AXIS2_PLACEMENT_3D('',#7162,#5682,#5683);
#5026=AXIS2_PLACEMENT_3D('',#7165,#5685,#5686);
#5027=AXIS2_PLACEMENT_3D('',#7166,#5687,#5688);
#5028=AXIS2_PLACEMENT_3D('',#7167,#5689,#5690);
#5029=AXIS2_PLACEMENT_3D('',#7169,#5691,#5692);
#5030=AXIS2_PLACEMENT_3D('',#7170,#5693,#5694);
#5031=AXIS2_PLACEMENT_3D('',#7172,#5695,#5696);
#5032=AXIS2_PLACEMENT_3D('',#7173,#5697,#5698);
#5033=AXIS2_PLACEMENT_3D('',#7177,#5700,#5701);
#5034=AXIS2_PLACEMENT_3D('',#7178,#5702,#5703);
#5035=AXIS2_PLACEMENT_3D('',#7182,#5705,#5706);
#5036=AXIS2_PLACEMENT_3D('',#7183,#5707,#5708);
#5037=AXIS2_PLACEMENT_3D('',#7185,#5709,#5710);
#5038=AXIS2_PLACEMENT_3D('',#7186,#5711,#5712);
#5039=AXIS2_PLACEMENT_3D('',#7187,#5713,#5714);
#5040=AXIS2_PLACEMENT_3D('',#7189,#5715,#5716);
#5041=AXIS2_PLACEMENT_3D('',#7190,#5717,#5718);
#5042=AXIS2_PLACEMENT_3D('',#7191,#5719,#5720);
#5043=AXIS2_PLACEMENT_3D('',#7192,#5721,#5722);
#5044=AXIS2_PLACEMENT_3D('',#7195,#5724,#5725);
#5045=AXIS2_PLACEMENT_3D('',#7196,#5726,#5727);
#5046=AXIS2_PLACEMENT_3D('',#7197,#5728,#5729);
#5047=AXIS2_PLACEMENT_3D('',#7235,#5732,#5733);
#5048=AXIS2_PLACEMENT_3D('',#7272,#5735,#5736);
#5049=AXIS2_PLACEMENT_3D('',#7313,#5738,#5739);
#5050=AXIS2_PLACEMENT_3D('',#7314,#5740,#5741);
#5051=AXIS2_PLACEMENT_3D('',#7316,#5742,#5743);
#5052=AXIS2_PLACEMENT_3D('',#7356,#5745,#5746);
#5053=AXIS2_PLACEMENT_3D('',#7357,#5747,#5748);
#5054=AXIS2_PLACEMENT_3D('',#7361,#5750,#5751);
#5055=AXIS2_PLACEMENT_3D('',#7362,#5752,#5753);
#5056=AXIS2_PLACEMENT_3D('',#7366,#5755,#5756);
#5057=AXIS2_PLACEMENT_3D('',#7367,#5757,#5758);
#5058=AXIS2_PLACEMENT_3D('',#7371,#5760,#5761);
#5059=AXIS2_PLACEMENT_3D('',#7372,#5762,#5763);
#5060=AXIS2_PLACEMENT_3D('',#7374,#5764,#5765);
#5061=AXIS2_PLACEMENT_3D('',#7375,#5766,#5767);
#5062=AXIS2_PLACEMENT_3D('',#7376,#5768,#5769);
#5063=AXIS2_PLACEMENT_3D('',#7378,#5770,#5771);
#5064=AXIS2_PLACEMENT_3D('',#7379,#5772,#5773);
#5065=AXIS2_PLACEMENT_3D('',#7380,#5774,#5775);
#5066=AXIS2_PLACEMENT_3D('',#7382,#5776,#5777);
#5067=AXIS2_PLACEMENT_3D('',#7385,#5779,#5780);
#5068=AXIS2_PLACEMENT_3D('',#7387,#5781,#5782);
#5069=AXIS2_PLACEMENT_3D('',#7391,#5785,#5786);
#5070=AXIS2_PLACEMENT_3D('',#7392,#5787,#5788);
#5071=AXIS2_PLACEMENT_3D('',#7393,#5789,#5790);
#5072=AXIS2_PLACEMENT_3D('',#7395,#5791,#5792);
#5073=AXIS2_PLACEMENT_3D('',#7396,#5793,#5794);
#5074=AXIS2_PLACEMENT_3D('',#7397,#5795,#5796);
#5075=AXIS2_PLACEMENT_3D('',#7399,#5797,#5798);
#5076=AXIS2_PLACEMENT_3D('',#7401,#5800,#5801);
#5077=AXIS2_PLACEMENT_3D('',#7445,#5803,#5804);
#5078=AXIS2_PLACEMENT_3D('',#7446,#5805,#5806);
#5079=AXIS2_PLACEMENT_3D('',#7447,#5807,#5808);
#5080=AXIS2_PLACEMENT_3D('',#7449,#5809,#5810);
#5081=AXIS2_PLACEMENT_3D('',#7452,#5812,#5813);
#5082=AXIS2_PLACEMENT_3D('',#7453,#5814,#5815);
#5083=AXIS2_PLACEMENT_3D('',#7455,#5816,#5817);
#5084=AXIS2_PLACEMENT_3D('',#7456,#5818,#5819);
#5085=AXIS2_PLACEMENT_3D('',#7458,#5820,#5821);
#5086=AXIS2_PLACEMENT_3D('',#7459,#5822,#5823);
#5087=AXIS2_PLACEMENT_3D('',#7461,#5824,#5825);
#5088=AXIS2_PLACEMENT_3D('',#7463,#5827,#5828);
#5089=AXIS2_PLACEMENT_3D('',#7466,#5830,#5831);
#5090=AXIS2_PLACEMENT_3D('',#7467,#5832,#5833);
#5091=AXIS2_PLACEMENT_3D('',#7469,#5834,#5835);
#5092=AXIS2_PLACEMENT_3D('',#7472,#5837,#5838);
#5093=AXIS2_PLACEMENT_3D('',#7473,#5839,#5840);
#5094=AXIS2_PLACEMENT_3D('',#7475,#5841,#5842);
#5095=AXIS2_PLACEMENT_3D('',#7476,#5843,#5844);
#5096=AXIS2_PLACEMENT_3D('',#7477,#5845,#5846);
#5097=AXIS2_PLACEMENT_3D('',#7479,#5847,#5848);
#5098=AXIS2_PLACEMENT_3D('',#7482,#5850,#5851);
#5099=AXIS2_PLACEMENT_3D('',#7483,#5852,#5853);
#5100=AXIS2_PLACEMENT_3D('',#7486,#5855,#5856);
#5101=AXIS2_PLACEMENT_3D('',#7487,#5857,#5858);
#5102=AXIS2_PLACEMENT_3D('',#7488,#5859,#5860);
#5103=AXIS2_PLACEMENT_3D('',#7490,#5861,#5862);
#5104=AXIS2_PLACEMENT_3D('',#7493,#5864,#5865);
#5105=AXIS2_PLACEMENT_3D('',#7494,#5866,#5867);
#5106=AXIS2_PLACEMENT_3D('',#7495,#5868,#5869);
#5107=AXIS2_PLACEMENT_3D('',#7497,#5870,#5871);
#5108=AXIS2_PLACEMENT_3D('',#7499,#5873,#5874);
#5109=AXIS2_PLACEMENT_3D('',#7500,#5875,#5876);
#5110=AXIS2_PLACEMENT_3D('',#7502,#5877,#5878);
#5111=AXIS2_PLACEMENT_3D('',#7506,#5881,#5882);
#5112=AXIS2_PLACEMENT_3D('',#7507,#5883,#5884);
#5113=AXIS2_PLACEMENT_3D('',#7508,#5885,#5886);
#5114=AXIS2_PLACEMENT_3D('',#7509,#5887,#5888);
#5115=AXIS2_PLACEMENT_3D('',#7510,#5889,#5890);
#5116=AXIS2_PLACEMENT_3D('',#7512,#5891,#5892);
#5117=AXIS2_PLACEMENT_3D('',#7513,#5893,#5894);
#5118=AXIS2_PLACEMENT_3D('',#7514,#5895,#5896);
#5119=AXIS2_PLACEMENT_3D('',#7515,#5897,#5898);
#5120=AXIS2_PLACEMENT_3D('',#7587,#5900,#5901);
#5121=AXIS2_PLACEMENT_3D('',#7659,#5903,#5904);
#5122=AXIS2_PLACEMENT_3D('',#7731,#5906,#5907);
#5123=AXIS2_PLACEMENT_3D('',#7803,#5909,#5910);
#5124=AXIS2_PLACEMENT_3D('',#7875,#5912,#5913);
#5125=AXIS2_PLACEMENT_3D('',#7947,#5915,#5916);
#5126=AXIS2_PLACEMENT_3D('',#8031,#5918,#5919);
#5127=AXIS2_PLACEMENT_3D('',#8109,#5921,#5922);
#5128=AXIS2_PLACEMENT_3D('',#8193,#5924,#5925);
#5129=AXIS2_PLACEMENT_3D('',#8271,#5927,#5928);
#5130=AXIS2_PLACEMENT_3D('',#8355,#5930,#5931);
#5131=AXIS2_PLACEMENT_3D('',#8433,#5933,#5934);
#5132=AXIS2_PLACEMENT_3D('',#8435,#5935,#5936);
#5133=AXIS2_PLACEMENT_3D('',#8441,#5941,#5942);
#5134=AXIS2_PLACEMENT_3D('',#8442,#5943,#5944);
#5135=AXIS2_PLACEMENT_3D('',#8443,#5945,#5946);
#5136=AXIS2_PLACEMENT_3D('',#8445,#5947,#5948);
#5137=AXIS2_PLACEMENT_3D('',#8448,#5950,#5951);
#5138=AXIS2_PLACEMENT_3D('',#8449,#5952,#5953);
#5139=AXIS2_PLACEMENT_3D('',#8450,#5954,#5955);
#5140=AXIS2_PLACEMENT_3D('',#8452,#5956,#5957);
#5141=AXIS2_PLACEMENT_3D('',#8458,#5962,#5963);
#5142=AXIS2_PLACEMENT_3D('',#8459,#5964,#5965);
#5143=AXIS2_PLACEMENT_3D('',#8460,#5966,#5967);
#5144=AXIS2_PLACEMENT_3D('',#8461,#5968,#5969);
#5145=AXIS2_PLACEMENT_3D('',#8462,#5970,#5971);
#5146=AXIS2_PLACEMENT_3D('',#8464,#5972,#5973);
#5147=AXIS2_PLACEMENT_3D('',#8466,#5974,#5975);
#5148=AXIS2_PLACEMENT_3D('',#8467,#5976,#5977);
#5149=AXIS2_PLACEMENT_3D('',#8470,#5979,#5980);
#5150=AXIS2_PLACEMENT_3D('',#8471,#5981,#5982);
#5151=AXIS2_PLACEMENT_3D('',#8472,#5983,#5984);
#5152=AXIS2_PLACEMENT_3D('',#8474,#5985,#5986);
#5153=AXIS2_PLACEMENT_3D('',#8476,#5988,#5989);
#5154=AXIS2_PLACEMENT_3D('',#8477,#5990,#5991);
#5155=AXIS2_PLACEMENT_3D('',#8479,#5992,#5993);
#5156=AXIS2_PLACEMENT_3D('',#8482,#5995,#5996);
#5157=AXIS2_PLACEMENT_3D('',#8483,#5997,#5998);
#5158=AXIS2_PLACEMENT_3D('',#8484,#5999,#6000);
#5159=AXIS2_PLACEMENT_3D('',#8485,#6001,#6002);
#5160=AXIS2_PLACEMENT_3D('',#8494,#6007,#6008);
#5161=AXIS2_PLACEMENT_3D('',#8500,#6012,#6013);
#5162=AXIS2_PLACEMENT_3D('',#8506,#6017,#6018);
#5163=AXIS2_PLACEMENT_3D('',#8512,#6022,#6023);
#5164=AXIS2_PLACEMENT_3D('',#8515,#6026,#6027);
#5165=AXIS2_PLACEMENT_3D('',#8516,#6028,#6029);
#5166=AXIS2_PLACEMENT_3D('',#8517,#6030,#6031);
#5167=AXIS2_PLACEMENT_3D('',#8518,#6032,#6033);
#5168=AXIS2_PLACEMENT_3D('',#8520,#6034,#6035);
#5169=AXIS2_PLACEMENT_3D('',#8523,#6037,#6038);
#5170=AXIS2_PLACEMENT_3D('',#8524,#6039,#6040);
#5171=AXIS2_PLACEMENT_3D('',#8526,#6041,#6042);
#5172=AXIS2_PLACEMENT_3D('',#8529,#6044,#6045);
#5173=AXIS2_PLACEMENT_3D('',#8530,#6046,#6047);
#5174=AXIS2_PLACEMENT_3D('',#8532,#6048,#6049);
#5175=AXIS2_PLACEMENT_3D('',#8535,#6051,#6052);
#5176=AXIS2_PLACEMENT_3D('',#8536,#6053,#6054);
#5177=AXIS2_PLACEMENT_3D('',#8538,#6055,#6056);
#5178=AXIS2_PLACEMENT_3D('',#8541,#6058,#6059);
#5179=AXIS2_PLACEMENT_3D('',#8542,#6060,#6061);
#5180=AXIS2_PLACEMENT_3D('',#8544,#6062,#6063);
#5181=AXIS2_PLACEMENT_3D('',#8547,#6065,#6066);
#5182=AXIS2_PLACEMENT_3D('',#8548,#6067,#6068);
#5183=AXIS2_PLACEMENT_3D('',#8550,#6069,#6070);
#5184=AXIS2_PLACEMENT_3D('',#8553,#6072,#6073);
#5185=AXIS2_PLACEMENT_3D('',#8554,#6074,#6075);
#5186=AXIS2_PLACEMENT_3D('',#8563,#6080,#6081);
#5187=AXIS2_PLACEMENT_3D('',#8572,#6086,#6087);
#5188=AXIS2_PLACEMENT_3D('',#8578,#6091,#6092);
#5189=AXIS2_PLACEMENT_3D('',#8584,#6096,#6097);
#5190=AXIS2_PLACEMENT_3D('',#8587,#6100,#6101);
#5191=AXIS2_PLACEMENT_3D('',#8589,#6102,#6103);
#5192=AXIS2_PLACEMENT_3D('',#8592,#6105,#6106);
#5193=AXIS2_PLACEMENT_3D('',#8593,#6107,#6108);
#5194=AXIS2_PLACEMENT_3D('',#8599,#6112,#6113);
#5195=AXIS2_PLACEMENT_3D('',#8605,#6117,#6118);
#5196=AXIS2_PLACEMENT_3D('',#8608,#6121,#6122);
#5197=AXIS2_PLACEMENT_3D('',#8609,#6123,#6124);
#5198=AXIS2_PLACEMENT_3D('',#8610,#6125,#6126);
#5199=AXIS2_PLACEMENT_3D('',#8611,#6127,#6128);
#5200=AXIS2_PLACEMENT_3D('',#8625,#6135,#6136);
#5201=AXIS2_PLACEMENT_3D('',#8626,#6137,#6138);
#5202=AXIS2_PLACEMENT_3D('',#8640,#6145,#6146);
#5203=AXIS2_PLACEMENT_3D('',#8641,#6147,#6148);
#5204=AXIS2_PLACEMENT_3D('',#8644,#6151,#6152);
#5205=AXIS2_PLACEMENT_3D('',#8646,#6154,#6155);
#5206=AXIS2_PLACEMENT_3D('',#8648,#6157,#6158);
#5207=AXIS2_PLACEMENT_3D('',#8650,#6160,#6161);
#5208=AXIS2_PLACEMENT_3D('',#8652,#6163,#6164);
#5209=AXIS2_PLACEMENT_3D('',#8653,#6165,#6166);
#5210=AXIS2_PLACEMENT_3D('',#8656,#6168,#6169);
#5211=AXIS2_PLACEMENT_3D('',#8657,#6170,#6171);
#5212=AXIS2_PLACEMENT_3D('',#8659,#6172,#6173);
#5213=AXIS2_PLACEMENT_3D('',#8661,#6174,#6175);
#5214=AXIS2_PLACEMENT_3D('',#8662,#6176,#6177);
#5215=AXIS2_PLACEMENT_3D('',#8664,#6179,#6180);
#5216=AXIS2_PLACEMENT_3D('',#8666,#6181,#6182);
#5217=AXIS2_PLACEMENT_3D('',#8668,#6184,#6185);
#5218=AXIS2_PLACEMENT_3D('',#8670,#6186,#6187);
#5219=AXIS2_PLACEMENT_3D('',#8672,#6189,#6190);
#5220=AXIS2_PLACEMENT_3D('',#8674,#6191,#6192);
#5221=AXIS2_PLACEMENT_3D('',#8675,#6193,#6194);
#5222=AXIS2_PLACEMENT_3D('',#8677,#6196,#6197);
#5223=AXIS2_PLACEMENT_3D('',#8678,#6198,#6199);
#5224=AXIS2_PLACEMENT_3D('',#8680,#6200,#6201);
#5225=AXIS2_PLACEMENT_3D('',#8683,#6203,#6204);
#5226=AXIS2_PLACEMENT_3D('',#8684,#6205,#6206);
#5227=AXIS2_PLACEMENT_3D('',#8686,#6207,#6208);
#5228=AXIS2_PLACEMENT_3D('',#8689,#6210,#6211);
#5229=AXIS2_PLACEMENT_3D('',#8690,#6212,#6213);
#5230=AXIS2_PLACEMENT_3D('',#8691,#6214,#6215);
#5231=AXIS2_PLACEMENT_3D('',#8692,#6216,#6217);
#5232=AXIS2_PLACEMENT_3D('',#8693,#6218,#6219);
#5233=AXIS2_PLACEMENT_3D('',#8695,#6220,#6221);
#5234=AXIS2_PLACEMENT_3D('',#8697,#6222,#6223);
#5235=AXIS2_PLACEMENT_3D('',#8698,#6224,#6225);
#5236=AXIS2_PLACEMENT_3D('',#8700,#6226,#6227);
#5237=AXIS2_PLACEMENT_3D('',#8702,#6229,#6230);
#5238=AXIS2_PLACEMENT_3D('',#8704,#6231,#6232);
#5239=AXIS2_PLACEMENT_3D('',#8706,#6233,#6234);
#5240=AXIS2_PLACEMENT_3D('',#8707,#6235,#6236);
#5241=AXIS2_PLACEMENT_3D('',#8709,#6237,#6238);
#5242=AXIS2_PLACEMENT_3D('',#8711,#6239,#6240);
#5243=AXIS2_PLACEMENT_3D('',#8712,#6241,#6242);
#5244=AXIS2_PLACEMENT_3D('',#8714,#6244,#6245);
#5245=AXIS2_PLACEMENT_3D('',#8717,#6247,#6248);
#5246=AXIS2_PLACEMENT_3D('',#8718,#6249,#6250);
#5247=AXIS2_PLACEMENT_3D('',#8720,#6252,#6253);
#5248=AXIS2_PLACEMENT_3D('',#8721,#6254,#6255);
#5249=AXIS2_PLACEMENT_3D('',#8723,#6256,#6257);
#5250=AXIS2_PLACEMENT_3D('',#8726,#6259,#6260);
#5251=AXIS2_PLACEMENT_3D('',#8727,#6261,#6262);
#5252=AXIS2_PLACEMENT_3D('',#8728,#6263,#6264);
#5253=AXIS2_PLACEMENT_3D('',#8729,#6265,#6266);
#5254=AXIS2_PLACEMENT_3D('',#8730,#6267,#6268);
#5255=AXIS2_PLACEMENT_3D('',#8732,#6269,#6270);
#5256=AXIS2_PLACEMENT_3D('',#8735,#6272,#6273);
#5257=AXIS2_PLACEMENT_3D('',#8736,#6274,#6275);
#5258=AXIS2_PLACEMENT_3D('',#8738,#6276,#6277);
#5259=AXIS2_PLACEMENT_3D('',#8741,#6279,#6280);
#5260=AXIS2_PLACEMENT_3D('',#8742,#6281,#6282);
#5261=AXIS2_PLACEMENT_3D('',#8743,#6283,#6284);
#5262=AXIS2_PLACEMENT_3D('',#8744,#6285,#6286);
#5263=AXIS2_PLACEMENT_3D('',#8745,#6287,#6288);
#5264=AXIS2_PLACEMENT_3D('',#8747,#6289,#6290);
#5265=AXIS2_PLACEMENT_3D('',#8750,#6292,#6293);
#5266=AXIS2_PLACEMENT_3D('',#8751,#6294,#6295);
#5267=AXIS2_PLACEMENT_3D('',#8753,#6296,#6297);
#5268=AXIS2_PLACEMENT_3D('',#8756,#6299,#6300);
#5269=AXIS2_PLACEMENT_3D('',#8757,#6301,#6302);
#5270=AXIS2_PLACEMENT_3D('',#8759,#6303,#6304);
#5271=AXIS2_PLACEMENT_3D('',#8762,#6306,#6307);
#5272=AXIS2_PLACEMENT_3D('',#8763,#6308,#6309);
#5273=AXIS2_PLACEMENT_3D('',#8765,#6310,#6311);
#5274=AXIS2_PLACEMENT_3D('',#8768,#6313,#6314);
#5275=AXIS2_PLACEMENT_3D('',#8769,#6315,#6316);
#5276=AXIS2_PLACEMENT_3D('',#8771,#6317,#6318);
#5277=AXIS2_PLACEMENT_3D('',#8774,#6320,#6321);
#5278=AXIS2_PLACEMENT_3D('',#8775,#6322,#6323);
#5279=AXIS2_PLACEMENT_3D('',#8777,#6324,#6325);
#5280=AXIS2_PLACEMENT_3D('',#8780,#6327,#6328);
#5281=AXIS2_PLACEMENT_3D('',#8781,#6329,#6330);
#5282=AXIS2_PLACEMENT_3D('',#8783,#6331,#6332);
#5283=AXIS2_PLACEMENT_3D('',#8786,#6334,#6335);
#5284=AXIS2_PLACEMENT_3D('',#8787,#6336,#6337);
#5285=AXIS2_PLACEMENT_3D('',#8789,#6338,#6339);
#5286=AXIS2_PLACEMENT_3D('',#8792,#6341,#6342);
#5287=AXIS2_PLACEMENT_3D('',#8793,#6343,#6344);
#5288=AXIS2_PLACEMENT_3D('',#8794,#6345,#6346);
#5289=AXIS2_PLACEMENT_3D('',#8795,#6347,#6348);
#5290=AXIS2_PLACEMENT_3D('',#8796,#6349,#6350);
#5291=AXIS2_PLACEMENT_3D('',#8798,#6351,#6352);
#5292=AXIS2_PLACEMENT_3D('',#8801,#6354,#6355);
#5293=AXIS2_PLACEMENT_3D('',#8802,#6356,#6357);
#5294=AXIS2_PLACEMENT_3D('',#8804,#6358,#6359);
#5295=AXIS2_PLACEMENT_3D('',#8807,#6361,#6362);
#5296=AXIS2_PLACEMENT_3D('',#8808,#6363,#6364);
#5297=AXIS2_PLACEMENT_3D('',#8809,#6365,#6366);
#5298=AXIS2_PLACEMENT_3D('',#8811,#6367,#6368);
#5299=AXIS2_PLACEMENT_3D('',#8812,#6369,#6370);
#5300=AXIS2_PLACEMENT_3D('',#8814,#6371,#6372);
#5301=AXIS2_PLACEMENT_3D('',#8817,#6374,#6375);
#5302=AXIS2_PLACEMENT_3D('',#8818,#6376,#6377);
#5303=AXIS2_PLACEMENT_3D('',#8821,#6379,#6380);
#5304=AXIS2_PLACEMENT_3D('',#8822,#6381,#6382);
#5305=AXIS2_PLACEMENT_3D('',#8823,#6383,#6384);
#5306=AXIS2_PLACEMENT_3D('',#8824,#6385,#6386);
#5307=AXIS2_PLACEMENT_3D('',#8825,#6387,#6388);
#5308=AXIS2_PLACEMENT_3D('',#8828,#6389,#6390);
#5309=AXIS2_PLACEMENT_3D('',#8829,#6391,#6392);
#5310=AXIS2_PLACEMENT_3D('',#8830,#6393,#6394);
#5311=AXIS2_PLACEMENT_3D('',#8834,#6396,#6397);
#5312=AXIS2_PLACEMENT_3D('',#8836,#6399,#6400);
#5313=AXIS2_PLACEMENT_3D('',#8841,#6402,#6403);
#5314=AXIS2_PLACEMENT_3D('',#8844,#6405,#6406);
#5315=AXIS2_PLACEMENT_3D('',#8845,#6407,#6408);
#5316=AXIS2_PLACEMENT_3D('',#8846,#6409,#6410);
#5317=AXIS2_PLACEMENT_3D('',#8847,#6411,#6412);
#5318=AXIS2_PLACEMENT_3D('',#8850,#6413,#6414);
#5319=AXIS2_PLACEMENT_3D('',#8851,#6415,#6416);
#5320=AXIS2_PLACEMENT_3D('',#8852,#6417,#6418);
#5321=AXIS2_PLACEMENT_3D('',#8856,#6420,#6421);
#5322=AXIS2_PLACEMENT_3D('',#8858,#6423,#6424);
#5323=AXIS2_PLACEMENT_3D('',#8861,#6425,#6426);
#5324=AXIS2_PLACEMENT_3D('',#8862,#6427,#6428);
#5325=AXIS2_PLACEMENT_3D('',#8863,#6429,#6430);
#5326=AXIS2_PLACEMENT_3D('',#8867,#6432,#6433);
#5327=AXIS2_PLACEMENT_3D('',#8869,#6435,#6436);
#5328=AXIS2_PLACEMENT_3D('',#8872,#6437,#6438);
#5329=AXIS2_PLACEMENT_3D('',#8873,#6439,#6440);
#5330=AXIS2_PLACEMENT_3D('',#8874,#6441,#6442);
#5331=AXIS2_PLACEMENT_3D('',#8878,#6444,#6445);
#5332=AXIS2_PLACEMENT_3D('',#8880,#6447,#6448);
#5333=AXIS2_PLACEMENT_3D('',#8885,#6450,#6451);
#5334=AXIS2_PLACEMENT_3D('',#8888,#6453,#6454);
#5335=AXIS2_PLACEMENT_3D('',#8889,#6455,#6456);
#5336=AXIS2_PLACEMENT_3D('',#8890,#6457,#6458);
#5337=AXIS2_PLACEMENT_3D('',#8891,#6459,#6460);
#5338=AXIS2_PLACEMENT_3D('',#8893,#6461,#6462);
#5339=AXIS2_PLACEMENT_3D('',#8896,#6464,#6465);
#5340=AXIS2_PLACEMENT_3D('',#8897,#6466,#6467);
#5341=AXIS2_PLACEMENT_3D('',#8898,#6468,#6469);
#5342=AXIS2_PLACEMENT_3D('',#8899,#6470,#6471);
#5343=AXIS2_PLACEMENT_3D('',#8900,#6472,#6473);
#5344=AXIS2_PLACEMENT_3D('',#8901,#6474,#6475);
#5345=AXIS2_PLACEMENT_3D('',#8902,#6476,#6477);
#5346=AXIS2_PLACEMENT_3D('',#8903,#6478,#6479);
#5347=AXIS2_PLACEMENT_3D('',#8905,#6480,#6481);
#5348=AXIS2_PLACEMENT_3D('',#8908,#6483,#6484);
#5349=AXIS2_PLACEMENT_3D('',#8909,#6485,#6486);
#5350=AXIS2_PLACEMENT_3D('',#8911,#6487,#6488);
#5351=AXIS2_PLACEMENT_3D('',#8914,#6490,#6491);
#5352=AXIS2_PLACEMENT_3D('',#8915,#6492,#6493);
#5353=AXIS2_PLACEMENT_3D('',#8917,#6494,#6495);
#5354=AXIS2_PLACEMENT_3D('',#8920,#6497,#6498);
#5355=AXIS2_PLACEMENT_3D('',#8921,#6499,#6500);
#5356=AXIS2_PLACEMENT_3D('',#8923,#6501,#6502);
#5357=AXIS2_PLACEMENT_3D('',#8926,#6504,#6505);
#5358=AXIS2_PLACEMENT_3D('',#8927,#6506,#6507);
#5359=AXIS2_PLACEMENT_3D('',#8929,#6508,#6509);
#5360=AXIS2_PLACEMENT_3D('',#8932,#6511,#6512);
#5361=AXIS2_PLACEMENT_3D('',#8933,#6513,#6514);
#5362=AXIS2_PLACEMENT_3D('',#8935,#6515,#6516);
#5363=AXIS2_PLACEMENT_3D('',#8938,#6518,#6519);
#5364=AXIS2_PLACEMENT_3D('',#8939,#6520,#6521);
#5365=AXIS2_PLACEMENT_3D('',#8941,#6522,#6523);
#5366=AXIS2_PLACEMENT_3D('',#8944,#6525,#6526);
#5367=AXIS2_PLACEMENT_3D('',#8945,#6527,#6528);
#5368=AXIS2_PLACEMENT_3D('',#8947,#6529,#6530);
#5369=AXIS2_PLACEMENT_3D('',#8950,#6532,#6533);
#5370=AXIS2_PLACEMENT_3D('',#8951,#6534,#6535);
#5371=AXIS2_PLACEMENT_3D('',#8952,#6536,#6537);
#5372=AXIS2_PLACEMENT_3D('',#8953,#6538,#6539);
#5373=AXIS2_PLACEMENT_3D('',#8955,#6540,#6541);
#5374=AXIS2_PLACEMENT_3D('',#8958,#6543,#6544);
#5375=AXIS2_PLACEMENT_3D('',#8959,#6545,#6546);
#5376=AXIS2_PLACEMENT_3D('',#8960,#6547,#6548);
#5377=AXIS2_PLACEMENT_3D('',#8961,#6549,#6550);
#5378=AXIS2_PLACEMENT_3D('',#9673,#6551,#6552);
#5379=AXIS2_PLACEMENT_3D('',#9746,#6553,#6554);
#5380=AXIS2_PLACEMENT_3D('',#9747,#6555,#6556);
#5381=AXIS2_PLACEMENT_3D('',#9748,#6557,#6558);
#5382=AXIS2_PLACEMENT_3D('',#9749,#6559,#6560);
#5383=AXIS2_PLACEMENT_3D('',#9750,#6561,#6562);
#5384=AXIS2_PLACEMENT_3D('',#9752,#6563,#6564);
#5385=AXIS2_PLACEMENT_3D('',#9755,#6566,#6567);
#5386=AXIS2_PLACEMENT_3D('',#9756,#6568,#6569);
#5387=AXIS2_PLACEMENT_3D('',#9757,#6570,#6571);
#5388=AXIS2_PLACEMENT_3D('',#9759,#6572,#6573);
#5389=AXIS2_PLACEMENT_3D('',#9762,#6575,#6576);
#5390=AXIS2_PLACEMENT_3D('',#9763,#6577,#6578);
#5391=AXIS2_PLACEMENT_3D('',#9764,#6579,#6580);
#5392=AXIS2_PLACEMENT_3D('',#9765,#6581,#6582);
#5393=AXIS2_PLACEMENT_3D('',#9766,#6583,#6584);
#5394=AXIS2_PLACEMENT_3D('',#9768,#6585,#6586);
#5395=AXIS2_PLACEMENT_3D('',#9771,#6588,#6589);
#5396=AXIS2_PLACEMENT_3D('',#9772,#6590,#6591);
#5397=AXIS2_PLACEMENT_3D('',#9773,#6592,#6593);
#5398=AXIS2_PLACEMENT_3D('',#9774,#6594,#6595);
#5399=AXIS2_PLACEMENT_3D('',#9775,#6596,#6597);
#5400=AXIS2_PLACEMENT_3D('',#9780,#6599,#6600);
#5401=AXIS2_PLACEMENT_3D('',#9781,#6601,#6602);
#5402=AXIS2_PLACEMENT_3D('',#9782,#6603,#6604);
#5403=AXIS2_PLACEMENT_3D('',#9795,#6605,#6606);
#5404=AXIS2_PLACEMENT_3D('',#9842,#6608,#6609);
#5405=AXIS2_PLACEMENT_3D('',#9844,#6611,#6612);
#5406=AXIS2_PLACEMENT_3D('',#9846,#6613,#6614);
#5407=AXIS2_PLACEMENT_3D('',#9849,#6616,#6617);
#5408=AXIS2_PLACEMENT_3D('',#9850,#6618,#6619);
#5409=AXIS2_PLACEMENT_3D('',#9852,#6620,#6621);
#5410=AXIS2_PLACEMENT_3D('',#9855,#6623,#6624);
#5411=AXIS2_PLACEMENT_3D('',#9856,#6625,#6626);
#5412=AXIS2_PLACEMENT_3D('',#9857,#6627,#6628);
#5413=AXIS2_PLACEMENT_3D('',#9858,#6629,#6630);
#5414=AXIS2_PLACEMENT_3D('',#9859,#6631,#6632);
#5415=AXIS2_PLACEMENT_3D('',#9861,#6633,#6634);
#5416=AXIS2_PLACEMENT_3D('',#9862,#6635,#6636);
#5417=AXIS2_PLACEMENT_3D('',#9864,#6637,#6638);
#5418=AXIS2_PLACEMENT_3D('',#9866,#6640,#6641);
#5419=AXIS2_PLACEMENT_3D('',#9868,#6642,#6643);
#5420=AXIS2_PLACEMENT_3D('',#9870,#6645,#6646);
#5421=AXIS2_PLACEMENT_3D('',#9872,#6647,#6648);
#5422=AXIS2_PLACEMENT_3D('',#9874,#6650,#6651);
#5423=AXIS2_PLACEMENT_3D('',#9876,#6652,#6653);
#5424=AXIS2_PLACEMENT_3D('',#9877,#6654,#6655);
#5425=AXIS2_PLACEMENT_3D('',#9879,#6656,#6657);
#5426=AXIS2_PLACEMENT_3D('',#9881,#6659,#6660);
#5427=AXIS2_PLACEMENT_3D('',#9883,#6661,#6662);
#5428=AXIS2_PLACEMENT_3D('',#9885,#6664,#6665);
#5429=AXIS2_PLACEMENT_3D('',#9887,#6666,#6667);
#5430=AXIS2_PLACEMENT_3D('',#9889,#6669,#6670);
#5431=AXIS2_PLACEMENT_3D('',#9890,#6671,#6672);
#5432=AXIS2_PLACEMENT_3D('',#9899,#6677,#6678);
#5433=AXIS2_PLACEMENT_3D('',#9905,#6682,#6683);
#5434=AXIS2_PLACEMENT_3D('',#9911,#6687,#6688);
#5435=AXIS2_PLACEMENT_3D('',#9917,#6692,#6693);
#5436=AXIS2_PLACEMENT_3D('',#9923,#6697,#6698);
#5437=AXIS2_PLACEMENT_3D('',#9926,#6701,#6702);
#5438=AXIS2_PLACEMENT_3D('',#9927,#6703,#6704);
#5439=AXIS2_PLACEMENT_3D('',#9928,#6705,#6706);
#5440=AXIS2_PLACEMENT_3D('',#9929,#6707,#6708);
#5441=AXIS2_PLACEMENT_3D('',#9931,#6709,#6710);
#5442=AXIS2_PLACEMENT_3D('',#9934,#6712,#6713);
#5443=AXIS2_PLACEMENT_3D('',#9935,#6714,#6715);
#5444=AXIS2_PLACEMENT_3D('',#9937,#6716,#6717);
#5445=AXIS2_PLACEMENT_3D('',#9940,#6719,#6720);
#5446=AXIS2_PLACEMENT_3D('',#9941,#6721,#6722);
#5447=AXIS2_PLACEMENT_3D('',#9942,#6723,#6724);
#5448=AXIS2_PLACEMENT_3D('',#9943,#6725,#6726);
#5449=AXIS2_PLACEMENT_3D('',#9944,#6727,#6728);
#5450=AXIS2_PLACEMENT_3D('',#9956,#6730,#6731);
#5451=AXIS2_PLACEMENT_3D('',#9972,#6732,#6733);
#5452=AXIS2_PLACEMENT_3D('',#9974,#6734,#6735);
#5453=AXIS2_PLACEMENT_3D('',#10000,#6737,#6738);
#5454=AXIS2_PLACEMENT_3D('',#10003,#6741,#6742);
#5455=AXIS2_PLACEMENT_3D('',#10005,#6744,#6745);
#5456=AXIS2_PLACEMENT_3D('',#10007,#6747,#6748);
#5457=AXIS2_PLACEMENT_3D('',#10009,#6749,#6750);
#5458=AXIS2_PLACEMENT_3D('',#10012,#6752,#6753);
#5459=AXIS2_PLACEMENT_3D('',#10013,#6754,#6755);
#5460=AXIS2_PLACEMENT_3D('',#10015,#6757,#6758);
#5461=AXIS2_PLACEMENT_3D('',#10017,#6760,#6761);
#5462=AXIS2_PLACEMENT_3D('',#10018,#6762,#6763);
#5463=AXIS2_PLACEMENT_3D('',#10019,#6764,#6765);
#5464=AXIS2_PLACEMENT_3D('',#10020,#6766,#6767);
#5465=AXIS2_PLACEMENT_3D('',#10021,#6768,#6769);
#5466=AXIS2_PLACEMENT_3D('',#10030,#6774,#6775);
#5467=AXIS2_PLACEMENT_3D('',#10036,#6779,#6780);
#5468=AXIS2_PLACEMENT_3D('',#10042,#6784,#6785);
#5469=AXIS2_PLACEMENT_3D('',#10048,#6789,#6790);
#5470=AXIS2_PLACEMENT_3D('',#10054,#6794,#6795);
#5471=AXIS2_PLACEMENT_3D('',#10057,#6798,#6799);
#5472=AXIS2_PLACEMENT_3D('',#10058,#6800,#6801);
#5473=AXIS2_PLACEMENT_3D('',#10060,#6802,#6803);
#5474=AXIS2_PLACEMENT_3D('',#10061,#6804,#6805);
#5475=AXIS2_PLACEMENT_3D('',#10063,#6806,#6807);
#5476=AXIS2_PLACEMENT_3D('',#10065,#6809,#6810);
#5477=AXIS2_PLACEMENT_3D('',#10067,#6811,#6812);
#5478=AXIS2_PLACEMENT_3D('',#10069,#6814,#6815);
#5479=AXIS2_PLACEMENT_3D('',#10071,#6816,#6817);
#5480=AXIS2_PLACEMENT_3D('',#10073,#6819,#6820);
#5481=AXIS2_PLACEMENT_3D('',#10074,#6821,#6822);
#5482=AXIS2_PLACEMENT_3D('',#10075,#6823,#6824);
#5483=AXIS2_PLACEMENT_3D('',#10077,#6825,#6826);
#5484=AXIS2_PLACEMENT_3D('',#10078,#6827,#6828);
#5485=AXIS2_PLACEMENT_3D('',#10079,#6829,#6830);
#5486=AXIS2_PLACEMENT_3D('',#10080,#6831,#6832);
#5487=AXIS2_PLACEMENT_3D('',#10082,#6833,#6834);
#5488=AXIS2_PLACEMENT_3D('',#10085,#6836,#6837);
#5489=AXIS2_PLACEMENT_3D('',#10086,#6838,#6839);
#5490=AXIS2_PLACEMENT_3D('',#10095,#6844,#6845);
#5491=AXIS2_PLACEMENT_3D('',#10101,#6849,#6850);
#5492=AXIS2_PLACEMENT_3D('',#10107,#6854,#6855);
#5493=AXIS2_PLACEMENT_3D('',#10110,#6858,#6859);
#5494=AXIS2_PLACEMENT_3D('',#10111,#6860,#6861);
#5495=AXIS2_PLACEMENT_3D('',#10112,#6862,#6863);
#5496=AXIS2_PLACEMENT_3D('',#10113,#6864,#6865);
#5497=AXIS2_PLACEMENT_3D('',#10115,#6866,#6867);
#5498=AXIS2_PLACEMENT_3D('',#10116,#6868,#6869);
#5499=AXIS2_PLACEMENT_3D('',#10118,#6870,#6871);
#5500=AXIS2_PLACEMENT_3D('',#10120,#6873,#6874);
#5501=AXIS2_PLACEMENT_3D('',#10122,#6875,#6876);
#5502=AXIS2_PLACEMENT_3D('',#10124,#6878,#6879);
#5503=AXIS2_PLACEMENT_3D('',#10126,#6880,#6881);
#5504=AXIS2_PLACEMENT_3D('',#10128,#6883,#6884);
#5505=AXIS2_PLACEMENT_3D('',#10130,#6885,#6886);
#5506=AXIS2_PLACEMENT_3D('',#10131,#6887,#6888);
#5507=AXIS2_PLACEMENT_3D('',#10133,#6889,#6890);
#5508=AXIS2_PLACEMENT_3D('',#10135,#6892,#6893);
#5509=AXIS2_PLACEMENT_3D('',#10137,#6894,#6895);
#5510=AXIS2_PLACEMENT_3D('',#10139,#6897,#6898);
#5511=AXIS2_PLACEMENT_3D('',#10141,#6899,#6900);
#5512=AXIS2_PLACEMENT_3D('',#10143,#6902,#6903);
#5513=AXIS2_PLACEMENT_3D('',#10144,#6904,#6905);
#5514=AXIS2_PLACEMENT_3D('',#10153,#6910,#6911);
#5515=AXIS2_PLACEMENT_3D('',#10159,#6915,#6916);
#5516=AXIS2_PLACEMENT_3D('',#10165,#6920,#6921);
#5517=AXIS2_PLACEMENT_3D('',#10171,#6925,#6926);
#5518=AXIS2_PLACEMENT_3D('',#10177,#6930,#6931);
#5519=AXIS2_PLACEMENT_3D('',#10180,#6934,#6935);
#5520=AXIS2_PLACEMENT_3D('',#10181,#6936,#6937);
#5521=AXIS2_PLACEMENT_3D('',#10182,#6938,#6939);
#5522=AXIS2_PLACEMENT_3D('',#10183,#6940,#6941);
#5523=AXIS2_PLACEMENT_3D('',#10184,#6942,#6943);
#5524=AXIS2_PLACEMENT_3D('',#10185,#6944,#6945);
#5525=AXIS2_PLACEMENT_3D('',#10186,#6946,#6947);
#5526=AXIS2_PLACEMENT_3D('',#10187,#6948,#6949);
#5527=AXIS2_PLACEMENT_3D('',#10188,#6950,#6951);
#5528=AXIS2_PLACEMENT_3D('',#10189,#6952,#6953);
#5529=AXIS2_PLACEMENT_3D('',#10190,#6954,#6955);
#5530=AXIS2_PLACEMENT_3D('',#10191,#6956,#6957);
#5531=AXIS2_PLACEMENT_3D('',#10192,#6958,#6959);
#5532=AXIS2_PLACEMENT_3D('',#10193,#6960,#6961);
#5533=AXIS2_PLACEMENT_3D('',#10194,#6962,#6963);
#5534=AXIS2_PLACEMENT_3D('',#10195,#6964,#6965);
#5535=AXIS2_PLACEMENT_3D('',#10196,#6966,#6967);
#5536=AXIS2_PLACEMENT_3D('',#10197,#6968,#6969);
#5537=AXIS2_PLACEMENT_3D('',#10198,#6970,#6971);
#5538=AXIS2_PLACEMENT_3D('',#10199,#6972,#6973);
#5539=AXIS2_PLACEMENT_3D('',#10200,#6974,#6975);
#5540=AXIS2_PLACEMENT_3D('',#10201,#6976,#6977);
#5541=AXIS2_PLACEMENT_3D('',#10202,#6978,#6979);
#5542=AXIS2_PLACEMENT_3D('',#10203,#6980,#6981);
#5543=AXIS2_PLACEMENT_3D('',#10204,#6982,#6983);
#5544=AXIS2_PLACEMENT_3D('',#10205,#6984,#6985);
#5545=AXIS2_PLACEMENT_3D('',#10206,#6986,#6987);
#5546=AXIS2_PLACEMENT_3D('',#10207,#6988,#6989);
#5547=AXIS2_PLACEMENT_3D('',#10208,#6990,#6991);
#5548=AXIS2_PLACEMENT_3D('',#10209,#6992,#6993);
#5549=AXIS2_PLACEMENT_3D('',#10210,#6994,#6995);
#5550=AXIS2_PLACEMENT_3D('',#10211,#6996,#6997);
#5551=AXIS2_PLACEMENT_3D('',#10212,#6998,#6999);
#5552=AXIS2_PLACEMENT_3D('',#10213,#7000,#7001);
#5553=AXIS2_PLACEMENT_3D('',#10214,#7002,#7003);
#5554=AXIS2_PLACEMENT_3D('',#10215,#7004,#7005);
#5555=AXIS2_PLACEMENT_3D('',#10216,#7006,#7007);
#5556=DIRECTION('axis',(0.,0.,1.));
#5557=DIRECTION('refdir',(1.,0.,0.));
#5558=DIRECTION('axis',(0.,0.,1.));
#5559=DIRECTION('refdir',(1.,0.,0.));
#5560=DIRECTION('center_axis',(0.,0.,1.));
#5561=DIRECTION('ref_axis',(1.,0.,0.));
#5562=DIRECTION('center_axis',(0.,0.,1.));
#5563=DIRECTION('ref_axis',(1.,0.,0.));
#5564=DIRECTION('',(0.,0.,1.));
#5565=DIRECTION('center_axis',(0.,0.,1.));
#5566=DIRECTION('ref_axis',(1.,0.,0.));
#5567=DIRECTION('center_axis',(0.,0.,1.));
#5568=DIRECTION('ref_axis',(1.,0.,0.));
#5569=DIRECTION('',(0.,0.,1.));
#5570=DIRECTION('center_axis',(0.,0.,1.));
#5571=DIRECTION('ref_axis',(1.,0.,0.));
#5572=DIRECTION('center_axis',(0.,0.,1.));
#5573=DIRECTION('ref_axis',(1.,0.,0.));
#5574=DIRECTION('center_axis',(0.,0.,1.));
#5575=DIRECTION('ref_axis',(1.,0.,0.));
#5576=DIRECTION('center_axis',(0.,0.,1.));
#5577=DIRECTION('ref_axis',(1.,0.,0.));
#5578=DIRECTION('',(0.,0.,1.));
#5579=DIRECTION('center_axis',(0.,0.,1.));
#5580=DIRECTION('ref_axis',(1.,0.,0.));
#5581=DIRECTION('center_axis',(0.,0.,1.));
#5582=DIRECTION('ref_axis',(1.,0.,0.));
#5583=DIRECTION('center_axis',(0.,0.,1.));
#5584=DIRECTION('ref_axis',(1.,0.,0.));
#5585=DIRECTION('center_axis',(0.,0.,1.));
#5586=DIRECTION('ref_axis',(1.,0.,0.));
#5587=DIRECTION('',(0.,0.,1.));
#5588=DIRECTION('center_axis',(0.,0.,1.));
#5589=DIRECTION('ref_axis',(1.,0.,0.));
#5590=DIRECTION('center_axis',(0.,0.,1.));
#5591=DIRECTION('ref_axis',(1.,0.,0.));
#5592=DIRECTION('center_axis',(0.,0.,1.));
#5593=DIRECTION('ref_axis',(1.,0.,0.));
#5594=DIRECTION('center_axis',(0.,0.,1.));
#5595=DIRECTION('ref_axis',(1.,0.,0.));
#5596=DIRECTION('',(0.,0.,1.));
#5597=DIRECTION('center_axis',(0.,0.,1.));
#5598=DIRECTION('ref_axis',(1.,0.,0.));
#5599=DIRECTION('center_axis',(0.,0.,1.));
#5600=DIRECTION('ref_axis',(1.,0.,0.));
#5601=DIRECTION('center_axis',(0.,0.,1.));
#5602=DIRECTION('ref_axis',(1.,0.,0.));
#5603=DIRECTION('center_axis',(0.,0.,1.));
#5604=DIRECTION('ref_axis',(1.,0.,0.));
#5605=DIRECTION('',(0.,0.,1.));
#5606=DIRECTION('center_axis',(0.,0.,1.));
#5607=DIRECTION('ref_axis',(1.,0.,0.));
#5608=DIRECTION('center_axis',(0.,0.,1.));
#5609=DIRECTION('ref_axis',(1.,0.,0.));
#5610=DIRECTION('center_axis',(0.,0.,1.));
#5611=DIRECTION('ref_axis',(1.,0.,0.));
#5612=DIRECTION('center_axis',(0.,0.,-1.));
#5613=DIRECTION('ref_axis',(1.,0.,0.));
#5614=DIRECTION('',(0.,0.,1.));
#5615=DIRECTION('center_axis',(0.,0.,-1.));
#5616=DIRECTION('ref_axis',(1.,0.,0.));
#5617=DIRECTION('center_axis',(0.,0.,1.));
#5618=DIRECTION('ref_axis',(1.,0.,0.));
#5619=DIRECTION('center_axis',(0.,0.,1.));
#5620=DIRECTION('ref_axis',(1.,0.,0.));
#5621=DIRECTION('',(0.,0.,1.));
#5622=DIRECTION('center_axis',(0.,0.,1.));
#5623=DIRECTION('ref_axis',(1.,0.,0.));
#5624=DIRECTION('center_axis',(0.,0.,1.));
#5625=DIRECTION('ref_axis',(1.,0.,0.));
#5626=DIRECTION('center_axis',(0.,0.,1.));
#5627=DIRECTION('ref_axis',(1.,0.,0.));
#5628=DIRECTION('center_axis',(0.,0.,1.));
#5629=DIRECTION('ref_axis',(1.,0.,0.));
#5630=DIRECTION('center_axis',(0.,0.,1.));
#5631=DIRECTION('ref_axis',(1.,0.,0.));
#5632=DIRECTION('',(-1.,0.,0.));
#5633=DIRECTION('center_axis',(0.,0.,1.));
#5634=DIRECTION('ref_axis',(1.,0.,0.));
#5635=DIRECTION('center_axis',(0.,0.,1.));
#5636=DIRECTION('ref_axis',(1.,0.,0.));
#5637=DIRECTION('center_axis',(0.,0.,1.));
#5638=DIRECTION('ref_axis',(1.,0.,0.));
#5639=DIRECTION('',(0.,0.,-1.));
#5640=DIRECTION('',(0.,0.,1.));
#5641=DIRECTION('',(0.,0.,1.));
#5642=DIRECTION('center_axis',(0.,0.,-1.));
#5643=DIRECTION('ref_axis',(1.,0.,0.));
#5644=DIRECTION('center_axis',(0.,0.,1.));
#5645=DIRECTION('ref_axis',(1.,0.,0.));
#5646=DIRECTION('center_axis',(0.,0.,1.));
#5647=DIRECTION('ref_axis',(1.,0.,0.));
#5648=DIRECTION('',(0.,0.,1.));
#5649=DIRECTION('center_axis',(0.,0.,-1.));
#5650=DIRECTION('ref_axis',(1.,0.,0.));
#5651=DIRECTION('center_axis',(0.,0.,1.));
#5652=DIRECTION('ref_axis',(1.,0.,0.));
#5653=DIRECTION('center_axis',(0.,0.,1.));
#5654=DIRECTION('ref_axis',(1.,0.,0.));
#5655=DIRECTION('center_axis',(0.,0.,1.));
#5656=DIRECTION('ref_axis',(1.,0.,0.));
#5657=DIRECTION('',(0.,0.,1.));
#5658=DIRECTION('center_axis',(0.,0.,-1.));
#5659=DIRECTION('ref_axis',(1.,0.,0.));
#5660=DIRECTION('center_axis',(0.,0.,1.));
#5661=DIRECTION('ref_axis',(1.,0.,0.));
#5662=DIRECTION('center_axis',(0.,0.,1.));
#5663=DIRECTION('ref_axis',(1.,0.,0.));
#5664=DIRECTION('center_axis',(0.,0.,1.));
#5665=DIRECTION('ref_axis',(1.,0.,0.));
#5666=DIRECTION('',(0.,0.,1.));
#5667=DIRECTION('center_axis',(0.,0.,-1.));
#5668=DIRECTION('ref_axis',(1.,0.,0.));
#5669=DIRECTION('center_axis',(0.,0.,1.));
#5670=DIRECTION('ref_axis',(1.,0.,0.));
#5671=DIRECTION('center_axis',(0.,0.,1.));
#5672=DIRECTION('ref_axis',(1.,0.,0.));
#5673=DIRECTION('center_axis',(0.,0.,1.));
#5674=DIRECTION('ref_axis',(1.,0.,0.));
#5675=DIRECTION('',(0.,0.,1.));
#5676=DIRECTION('center_axis',(0.,0.,-1.));
#5677=DIRECTION('ref_axis',(1.,0.,0.));
#5678=DIRECTION('center_axis',(0.,0.,1.));
#5679=DIRECTION('ref_axis',(1.,0.,0.));
#5680=DIRECTION('center_axis',(0.,0.,1.));
#5681=DIRECTION('ref_axis',(1.,0.,0.));
#5682=DIRECTION('center_axis',(0.,0.,1.));
#5683=DIRECTION('ref_axis',(1.,0.,0.));
#5684=DIRECTION('',(0.,0.,1.));
#5685=DIRECTION('center_axis',(0.,0.,-1.));
#5686=DIRECTION('ref_axis',(1.,0.,0.));
#5687=DIRECTION('center_axis',(0.,0.,1.));
#5688=DIRECTION('ref_axis',(1.,0.,0.));
#5689=DIRECTION('center_axis',(0.,1.,0.));
#5690=DIRECTION('ref_axis',(1.,0.,0.));
#5691=DIRECTION('center_axis',(0.,1.,0.));
#5692=DIRECTION('ref_axis',(1.,0.,0.));
#5693=DIRECTION('center_axis',(0.,1.,0.));
#5694=DIRECTION('ref_axis',(1.,0.,0.));
#5695=DIRECTION('center_axis',(0.,1.,0.));
#5696=DIRECTION('ref_axis',(1.,0.,0.));
#5697=DIRECTION('center_axis',(0.,0.,1.));
#5698=DIRECTION('ref_axis',(1.,0.,0.));
#5699=DIRECTION('',(0.,-1.,0.));
#5700=DIRECTION('center_axis',(0.,0.,1.));
#5701=DIRECTION('ref_axis',(1.,0.,0.));
#5702=DIRECTION('center_axis',(0.,0.,1.));
#5703=DIRECTION('ref_axis',(1.,0.,0.));
#5704=DIRECTION('',(0.,1.,0.));
#5705=DIRECTION('center_axis',(0.,0.,1.));
#5706=DIRECTION('ref_axis',(1.,0.,0.));
#5707=DIRECTION('center_axis',(0.,0.,1.));
#5708=DIRECTION('ref_axis',(-1.,1.22464679914735E-16,0.));
#5709=DIRECTION('center_axis',(0.,-0.707106781186548,-0.707106781186547));
#5710=DIRECTION('ref_axis',(0.,0.707106781186547,-0.707106781186548));
#5711=DIRECTION('center_axis',(0.,0.707106781186548,-0.707106781186547));
#5712=DIRECTION('ref_axis',(0.,0.707106781186547,0.707106781186548));
#5713=DIRECTION('center_axis',(0.,0.,1.));
#5714=DIRECTION('ref_axis',(1.,0.,0.));
#5715=DIRECTION('center_axis',(0.,0.707106781186548,-0.707106781186547));
#5716=DIRECTION('ref_axis',(0.,0.707106781186547,0.707106781186548));
#5717=DIRECTION('center_axis',(0.,-0.707106781186548,-0.707106781186547));
#5718=DIRECTION('ref_axis',(0.,0.707106781186547,-0.707106781186548));
#5719=DIRECTION('center_axis',(0.,0.,1.));
#5720=DIRECTION('ref_axis',(1.,0.,0.));
#5721=DIRECTION('center_axis',(0.,0.707106781186548,0.707106781186547));
#5722=DIRECTION('ref_axis',(0.,0.707106781186547,-0.707106781186548));
#5723=DIRECTION('',(0.,0.,1.));
#5724=DIRECTION('center_axis',(0.,0.,-1.));
#5725=DIRECTION('ref_axis',(1.,0.,0.));
#5726=DIRECTION('center_axis',(0.,-0.707106781186548,0.707106781186547));
#5727=DIRECTION('ref_axis',(0.,0.707106781186547,0.707106781186548));
#5728=DIRECTION('center_axis',(0.,1.,0.));
#5729=DIRECTION('ref_axis',(1.,0.,0.));
#5730=DIRECTION('',(0.,1.,0.));
#5731=DIRECTION('',(0.,1.,0.));
#5732=DIRECTION('center_axis',(0.,1.,0.));
#5733=DIRECTION('ref_axis',(1.,0.,0.));
#5734=DIRECTION('',(0.,1.,0.));
#5735=DIRECTION('center_axis',(1.,0.,0.));
#5736=DIRECTION('ref_axis',(0.,0.,-1.));
#5737=DIRECTION('',(1.,0.,0.));
#5738=DIRECTION('center_axis',(-1.,0.,0.));
#5739=DIRECTION('ref_axis',(0.,0.,-1.));
#5740=DIRECTION('center_axis',(1.,0.,0.));
#5741=DIRECTION('ref_axis',(0.,0.,-1.));
#5742=DIRECTION('center_axis',(1.,0.,0.));
#5743=DIRECTION('ref_axis',(0.,0.,-1.));
#5744=DIRECTION('',(1.,0.,0.));
#5745=DIRECTION('center_axis',(1.,0.,0.));
#5746=DIRECTION('ref_axis',(0.,0.,-1.));
#5747=DIRECTION('center_axis',(0.,0.,1.));
#5748=DIRECTION('ref_axis',(1.,0.,0.));
#5749=DIRECTION('',(-1.,0.,0.));
#5750=DIRECTION('center_axis',(0.,0.,1.));
#5751=DIRECTION('ref_axis',(1.,0.,0.));
#5752=DIRECTION('center_axis',(0.,0.,1.));
#5753=DIRECTION('ref_axis',(1.,0.,0.));
#5754=DIRECTION('',(1.,0.,0.));
#5755=DIRECTION('center_axis',(0.,0.,1.));
#5756=DIRECTION('ref_axis',(1.,0.,0.));
#5757=DIRECTION('center_axis',(0.,0.,1.));
#5758=DIRECTION('ref_axis',(1.,0.,0.));
#5759=DIRECTION('',(0.,-1.,0.));
#5760=DIRECTION('center_axis',(0.,0.,1.));
#5761=DIRECTION('ref_axis',(1.,0.,0.));
#5762=DIRECTION('center_axis',(0.,0.,1.));
#5763=DIRECTION('ref_axis',(1.,0.,0.));
#5764=DIRECTION('center_axis',(0.707106781186547,0.,0.707106781186548));
#5765=DIRECTION('ref_axis',(0.707106781186548,0.,-0.707106781186547));
#5766=DIRECTION('center_axis',(-0.707106781186547,0.,0.707106781186548));
#5767=DIRECTION('ref_axis',(0.707106781186548,0.,0.707106781186547));
#5768=DIRECTION('center_axis',(0.,0.,1.));
#5769=DIRECTION('ref_axis',(1.,0.,0.));
#5770=DIRECTION('center_axis',(-0.707106781186547,0.,0.707106781186548));
#5771=DIRECTION('ref_axis',(0.707106781186548,0.,0.707106781186547));
#5772=DIRECTION('center_axis',(0.707106781186547,0.,0.707106781186548));
#5773=DIRECTION('ref_axis',(0.707106781186548,0.,-0.707106781186547));
#5774=DIRECTION('center_axis',(0.,0.,1.));
#5775=DIRECTION('ref_axis',(1.,0.,0.));
#5776=DIRECTION('center_axis',(0.,0.,1.));
#5777=DIRECTION('ref_axis',(1.,0.,0.));
#5778=DIRECTION('',(0.,0.,1.));
#5779=DIRECTION('center_axis',(0.707106781186547,0.,-0.707106781186548));
#5780=DIRECTION('ref_axis',(0.707106781186548,0.,0.707106781186547));
#5781=DIRECTION('center_axis',(-0.707106781186547,0.,-0.707106781186548));
#5782=DIRECTION('ref_axis',(0.707106781186548,0.,-0.707106781186547));
#5783=DIRECTION('',(0.,0.,-1.));
#5784=DIRECTION('',(0.,0.,1.));
#5785=DIRECTION('center_axis',(-0.707106781186547,0.,-0.707106781186548));
#5786=DIRECTION('ref_axis',(0.707106781186548,0.,-0.707106781186547));
#5787=DIRECTION('center_axis',(0.707106781186547,0.,-0.707106781186548));
#5788=DIRECTION('ref_axis',(0.707106781186548,0.,0.707106781186547));
#5789=DIRECTION('center_axis',(1.,0.,0.));
#5790=DIRECTION('ref_axis',(0.,0.,-1.));
#5791=DIRECTION('center_axis',(1.,0.,0.));
#5792=DIRECTION('ref_axis',(0.,0.,-1.));
#5793=DIRECTION('center_axis',(1.,0.,0.));
#5794=DIRECTION('ref_axis',(0.,0.,-1.));
#5795=DIRECTION('center_axis',(1.,0.,0.));
#5796=DIRECTION('ref_axis',(0.,0.,-1.));
#5797=DIRECTION('center_axis',(1.,0.,0.));
#5798=DIRECTION('ref_axis',(0.,0.,-1.));
#5799=DIRECTION('',(1.,0.,0.));
#5800=DIRECTION('center_axis',(1.,0.,0.));
#5801=DIRECTION('ref_axis',(0.,0.,-1.));
#5802=DIRECTION('',(1.,0.,0.));
#5803=DIRECTION('center_axis',(1.,0.,0.));
#5804=DIRECTION('ref_axis',(0.,0.,-1.));
#5805=DIRECTION('center_axis',(1.,0.,0.));
#5806=DIRECTION('ref_axis',(0.,0.,-1.));
#5807=DIRECTION('center_axis',(0.,0.,1.));
#5808=DIRECTION('ref_axis',(1.,0.,0.));
#5809=DIRECTION('center_axis',(0.,0.,1.));
#5810=DIRECTION('ref_axis',(1.,0.,0.));
#5811=DIRECTION('',(0.,0.,1.));
#5812=DIRECTION('center_axis',(0.,0.,1.));
#5813=DIRECTION('ref_axis',(1.,0.,0.));
#5814=DIRECTION('center_axis',(0.,0.,1.));
#5815=DIRECTION('ref_axis',(1.,0.,0.));
#5816=DIRECTION('center_axis',(0.,0.,-1.));
#5817=DIRECTION('ref_axis',(1.,0.,0.));
#5818=DIRECTION('center_axis',(0.,0.,1.));
#5819=DIRECTION('ref_axis',(1.,0.,0.));
#5820=DIRECTION('center_axis',(0.,0.,1.));
#5821=DIRECTION('ref_axis',(1.,0.,0.));
#5822=DIRECTION('center_axis',(0.,0.,1.));
#5823=DIRECTION('ref_axis',(1.,0.,0.));
#5824=DIRECTION('center_axis',(0.,0.,1.));
#5825=DIRECTION('ref_axis',(1.,0.,0.));
#5826=DIRECTION('',(0.,0.,1.));
#5827=DIRECTION('center_axis',(0.,0.,1.));
#5828=DIRECTION('ref_axis',(1.,0.,0.));
#5829=DIRECTION('',(0.,0.,1.));
#5830=DIRECTION('center_axis',(0.,0.,-1.));
#5831=DIRECTION('ref_axis',(1.,0.,0.));
#5832=DIRECTION('center_axis',(0.,0.,1.));
#5833=DIRECTION('ref_axis',(1.,0.,0.));
#5834=DIRECTION('center_axis',(0.,0.,1.));
#5835=DIRECTION('ref_axis',(1.,0.,0.));
#5836=DIRECTION('',(0.,0.,-1.));
#5837=DIRECTION('center_axis',(0.,0.,1.));
#5838=DIRECTION('ref_axis',(1.,0.,0.));
#5839=DIRECTION('center_axis',(0.,0.,1.));
#5840=DIRECTION('ref_axis',(1.,0.,0.));
#5841=DIRECTION('center_axis',(0.,0.,-1.));
#5842=DIRECTION('ref_axis',(1.,0.,0.));
#5843=DIRECTION('center_axis',(0.,0.,1.));
#5844=DIRECTION('ref_axis',(1.,0.,0.));
#5845=DIRECTION('center_axis',(0.,0.,1.));
#5846=DIRECTION('ref_axis',(1.,0.,0.));
#5847=DIRECTION('center_axis',(0.,0.,1.));
#5848=DIRECTION('ref_axis',(1.,0.,0.));
#5849=DIRECTION('',(0.,0.,1.));
#5850=DIRECTION('center_axis',(0.,0.,-1.));
#5851=DIRECTION('ref_axis',(1.,0.,0.));
#5852=DIRECTION('center_axis',(0.,0.,1.));
#5853=DIRECTION('ref_axis',(1.,0.,0.));
#5854=DIRECTION('',(0.,0.,1.));
#5855=DIRECTION('center_axis',(0.,0.,1.));
#5856=DIRECTION('ref_axis',(1.,0.,0.));
#5857=DIRECTION('center_axis',(0.,0.,1.));
#5858=DIRECTION('ref_axis',(1.,0.,0.));
#5859=DIRECTION('center_axis',(0.,0.,1.));
#5860=DIRECTION('ref_axis',(1.,0.,0.));
#5861=DIRECTION('center_axis',(0.,0.,1.));
#5862=DIRECTION('ref_axis',(1.,0.,0.));
#5863=DIRECTION('',(0.,0.,1.));
#5864=DIRECTION('center_axis',(0.,0.,-1.));
#5865=DIRECTION('ref_axis',(1.,0.,0.));
#5866=DIRECTION('center_axis',(0.,0.,1.));
#5867=DIRECTION('ref_axis',(1.,0.,0.));
#5868=DIRECTION('center_axis',(0.,0.,1.));
#5869=DIRECTION('ref_axis',(1.,0.,0.));
#5870=DIRECTION('center_axis',(0.,0.,1.));
#5871=DIRECTION('ref_axis',(1.,0.,0.));
#5872=DIRECTION('',(0.,0.,1.));
#5873=DIRECTION('center_axis',(0.,0.,1.));
#5874=DIRECTION('ref_axis',(1.,0.,0.));
#5875=DIRECTION('center_axis',(0.,0.,1.));
#5876=DIRECTION('ref_axis',(1.,0.,0.));
#5877=DIRECTION('center_axis',(0.,0.,1.));
#5878=DIRECTION('ref_axis',(1.,0.,0.));
#5879=DIRECTION('',(0.,0.,-1.));
#5880=DIRECTION('',(0.,0.,-1.));
#5881=DIRECTION('center_axis',(0.,0.,1.));
#5882=DIRECTION('ref_axis',(1.,0.,0.));
#5883=DIRECTION('center_axis',(0.,0.,1.));
#5884=DIRECTION('ref_axis',(1.,0.,0.));
#5885=DIRECTION('center_axis',(0.,0.,1.));
#5886=DIRECTION('ref_axis',(1.,0.,0.));
#5887=DIRECTION('axis',(0.,0.,1.));
#5888=DIRECTION('refdir',(1.,0.,0.));
#5889=DIRECTION('center_axis',(0.,0.,1.));
#5890=DIRECTION('ref_axis',(1.,0.,0.));
#5891=DIRECTION('center_axis',(1.22464679914735E-16,-1.,0.));
#5892=DIRECTION('ref_axis',(-1.,-1.22464679914735E-16,0.));
#5893=DIRECTION('center_axis',(0.,0.,-1.));
#5894=DIRECTION('ref_axis',(1.,0.,0.));
#5895=DIRECTION('axis',(0.,0.,1.));
#5896=DIRECTION('refdir',(1.,0.,0.));
#5897=DIRECTION('center_axis',(0.,1.,0.));
#5898=DIRECTION('ref_axis',(1.,0.,0.));
#5899=DIRECTION('',(0.,1.,0.));
#5900=DIRECTION('center_axis',(0.,1.,0.));
#5901=DIRECTION('ref_axis',(1.,0.,0.));
#5902=DIRECTION('',(0.,1.,0.));
#5903=DIRECTION('center_axis',(0.,1.,0.));
#5904=DIRECTION('ref_axis',(1.,0.,0.));
#5905=DIRECTION('',(0.,1.,0.));
#5906=DIRECTION('center_axis',(0.,1.,0.));
#5907=DIRECTION('ref_axis',(1.,0.,0.));
#5908=DIRECTION('',(0.,1.,0.));
#5909=DIRECTION('center_axis',(0.,1.,0.));
#5910=DIRECTION('ref_axis',(1.,0.,0.));
#5911=DIRECTION('',(0.,1.,0.));
#5912=DIRECTION('center_axis',(0.,1.,0.));
#5913=DIRECTION('ref_axis',(1.,0.,0.));
#5914=DIRECTION('',(0.,1.,0.));
#5915=DIRECTION('center_axis',(1.,0.,0.));
#5916=DIRECTION('ref_axis',(0.,0.,-1.));
#5917=DIRECTION('',(1.,0.,0.));
#5918=DIRECTION('center_axis',(1.,0.,0.));
#5919=DIRECTION('ref_axis',(0.,0.,-1.));
#5920=DIRECTION('',(1.,0.,0.));
#5921=DIRECTION('center_axis',(1.,0.,0.));
#5922=DIRECTION('ref_axis',(0.,0.,-1.));
#5923=DIRECTION('',(1.,0.,0.));
#5924=DIRECTION('center_axis',(1.,0.,0.));
#5925=DIRECTION('ref_axis',(0.,0.,-1.));
#5926=DIRECTION('',(1.,0.,0.));
#5927=DIRECTION('center_axis',(1.,0.,0.));
#5928=DIRECTION('ref_axis',(0.,0.,-1.));
#5929=DIRECTION('',(1.,0.,0.));
#5930=DIRECTION('center_axis',(1.,0.,0.));
#5931=DIRECTION('ref_axis',(0.,0.,-1.));
#5932=DIRECTION('',(1.,0.,0.));
#5933=DIRECTION('center_axis',(0.,0.,1.));
#5934=DIRECTION('ref_axis',(1.,0.,0.));
#5935=DIRECTION('center_axis',(0.,0.,1.));
#5936=DIRECTION('ref_axis',(1.,0.,0.));
#5937=DIRECTION('',(0.,0.,1.));
#5938=DIRECTION('',(0.,0.,1.));
#5939=DIRECTION('',(0.,0.,1.));
#5940=DIRECTION('',(0.,0.,1.));
#5941=DIRECTION('center_axis',(0.,0.,-1.));
#5942=DIRECTION('ref_axis',(1.,0.,0.));
#5943=DIRECTION('center_axis',(0.,0.,1.));
#5944=DIRECTION('ref_axis',(1.,0.,0.));
#5945=DIRECTION('center_axis',(0.,0.,1.));
#5946=DIRECTION('ref_axis',(1.,0.,0.));
#5947=DIRECTION('center_axis',(0.,0.,1.));
#5948=DIRECTION('ref_axis',(1.,0.,0.));
#5949=DIRECTION('',(0.,0.,-1.));
#5950=DIRECTION('center_axis',(0.,0.,-1.));
#5951=DIRECTION('ref_axis',(1.,0.,0.));
#5952=DIRECTION('center_axis',(0.,0.,1.));
#5953=DIRECTION('ref_axis',(1.,0.,0.));
#5954=DIRECTION('center_axis',(0.,0.,1.));
#5955=DIRECTION('ref_axis',(1.,0.,0.));
#5956=DIRECTION('center_axis',(0.,0.,1.));
#5957=DIRECTION('ref_axis',(1.,0.,0.));
#5958=DIRECTION('',(0.,0.,-1.));
#5959=DIRECTION('',(0.,0.,-1.));
#5960=DIRECTION('',(0.,0.,-1.));
#5961=DIRECTION('',(0.,0.,-1.));
#5962=DIRECTION('center_axis',(0.,0.,1.));
#5963=DIRECTION('ref_axis',(1.,0.,0.));
#5964=DIRECTION('center_axis',(0.,0.,1.));
#5965=DIRECTION('ref_axis',(1.,0.,0.));
#5966=DIRECTION('center_axis',(0.,0.,1.));
#5967=DIRECTION('ref_axis',(1.,0.,0.));
#5968=DIRECTION('axis',(0.,0.,1.));
#5969=DIRECTION('refdir',(1.,0.,0.));
#5970=DIRECTION('center_axis',(0.,1.,0.));
#5971=DIRECTION('ref_axis',(1.,0.,0.));
#5972=DIRECTION('center_axis',(0.,1.,0.));
#5973=DIRECTION('ref_axis',(1.,0.,0.));
#5974=DIRECTION('center_axis',(0.,1.,0.));
#5975=DIRECTION('ref_axis',(1.,0.,0.));
#5976=DIRECTION('center_axis',(0.,1.,0.));
#5977=DIRECTION('ref_axis',(1.,0.,0.));
#5978=DIRECTION('',(0.,-1.,0.));
#5979=DIRECTION('center_axis',(0.,1.,0.));
#5980=DIRECTION('ref_axis',(1.,0.,0.));
#5981=DIRECTION('center_axis',(0.,1.,0.));
#5982=DIRECTION('ref_axis',(1.,0.,0.));
#5983=DIRECTION('center_axis',(0.,1.,0.));
#5984=DIRECTION('ref_axis',(1.,0.,0.));
#5985=DIRECTION('center_axis',(0.,1.,0.));
#5986=DIRECTION('ref_axis',(1.,0.,0.));
#5987=DIRECTION('',(0.,-1.,0.));
#5988=DIRECTION('center_axis',(0.,1.,0.));
#5989=DIRECTION('ref_axis',(1.,0.,0.));
#5990=DIRECTION('center_axis',(0.,1.,0.));
#5991=DIRECTION('ref_axis',(1.,0.,0.));
#5992=DIRECTION('center_axis',(0.,1.,0.));
#5993=DIRECTION('ref_axis',(1.,0.,0.));
#5994=DIRECTION('',(0.,-1.,0.));
#5995=DIRECTION('center_axis',(0.,1.,0.));
#5996=DIRECTION('ref_axis',(1.,0.,0.));
#5997=DIRECTION('center_axis',(0.,1.,0.));
#5998=DIRECTION('ref_axis',(1.,0.,0.));
#5999=DIRECTION('center_axis',(0.,1.,0.));
#6000=DIRECTION('ref_axis',(1.,0.,0.));
#6001=DIRECTION('center_axis',(-1.,0.,0.));
#6002=DIRECTION('ref_axis',(0.,0.,1.));
#6003=DIRECTION('',(0.,0.,-1.));
#6004=DIRECTION('',(0.,1.,0.));
#6005=DIRECTION('',(0.,0.,1.));
#6006=DIRECTION('',(0.,1.,0.));
#6007=DIRECTION('center_axis',(0.,0.,-1.));
#6008=DIRECTION('ref_axis',(-1.,0.,0.));
#6009=DIRECTION('',(1.,0.,0.));
#6010=DIRECTION('',(-1.,0.,0.));
#6011=DIRECTION('',(0.,1.,0.));
#6012=DIRECTION('center_axis',(1.,0.,0.));
#6013=DIRECTION('ref_axis',(0.,0.,-1.));
#6014=DIRECTION('',(0.,0.,1.));
#6015=DIRECTION('',(0.,0.,-1.));
#6016=DIRECTION('',(0.,1.,0.));
#6017=DIRECTION('center_axis',(0.986393923832144,0.,0.164398987305357));
#6018=DIRECTION('ref_axis',(0.164398987305357,0.,-0.986393923832144));
#6019=DIRECTION('',(-0.164398987305357,0.,0.986393923832144));
#6020=DIRECTION('',(0.164398987305357,0.,-0.986393923832144));
#6021=DIRECTION('',(0.,1.,0.));
#6022=DIRECTION('center_axis',(-0.986393923832144,0.,0.164398987305357));
#6023=DIRECTION('ref_axis',(0.164398987305357,0.,0.986393923832144));
#6024=DIRECTION('',(-0.164398987305357,0.,-0.986393923832144));
#6025=DIRECTION('',(0.164398987305357,0.,0.986393923832144));
#6026=DIRECTION('center_axis',(0.,1.,0.));
#6027=DIRECTION('ref_axis',(0.,0.,1.));
#6028=DIRECTION('center_axis',(0.,1.,0.));
#6029=DIRECTION('ref_axis',(1.,0.,0.));
#6030=DIRECTION('axis',(0.,0.,1.));
#6031=DIRECTION('refdir',(1.,0.,0.));
#6032=DIRECTION('center_axis',(0.,0.,1.));
#6033=DIRECTION('ref_axis',(1.,0.,0.));
#6034=DIRECTION('center_axis',(0.,0.,1.));
#6035=DIRECTION('ref_axis',(1.,0.,0.));
#6036=DIRECTION('',(0.,0.,1.));
#6037=DIRECTION('center_axis',(0.,0.,-1.));
#6038=DIRECTION('ref_axis',(1.,0.,0.));
#6039=DIRECTION('center_axis',(0.,0.,1.));
#6040=DIRECTION('ref_axis',(1.,0.,0.));
#6041=DIRECTION('center_axis',(0.,0.,1.));
#6042=DIRECTION('ref_axis',(1.,0.,0.));
#6043=DIRECTION('',(0.,0.,1.));
#6044=DIRECTION('center_axis',(0.,0.,-1.));
#6045=DIRECTION('ref_axis',(1.,0.,0.));
#6046=DIRECTION('center_axis',(0.,1.,0.));
#6047=DIRECTION('ref_axis',(1.,0.,0.));
#6048=DIRECTION('center_axis',(0.,1.,0.));
#6049=DIRECTION('ref_axis',(1.,0.,0.));
#6050=DIRECTION('',(0.,1.,0.));
#6051=DIRECTION('center_axis',(0.,-1.,0.));
#6052=DIRECTION('ref_axis',(1.,0.,0.));
#6053=DIRECTION('center_axis',(0.,1.,0.));
#6054=DIRECTION('ref_axis',(1.,0.,0.));
#6055=DIRECTION('center_axis',(0.,1.,0.));
#6056=DIRECTION('ref_axis',(1.,0.,0.));
#6057=DIRECTION('',(0.,1.,0.));
#6058=DIRECTION('center_axis',(0.,-1.,0.));
#6059=DIRECTION('ref_axis',(1.,0.,0.));
#6060=DIRECTION('center_axis',(0.,1.,0.));
#6061=DIRECTION('ref_axis',(1.,0.,0.));
#6062=DIRECTION('center_axis',(0.,1.,0.));
#6063=DIRECTION('ref_axis',(1.,0.,0.));
#6064=DIRECTION('',(0.,1.,0.));
#6065=DIRECTION('center_axis',(0.,-1.,0.));
#6066=DIRECTION('ref_axis',(1.,0.,0.));
#6067=DIRECTION('center_axis',(0.,1.,0.));
#6068=DIRECTION('ref_axis',(1.,0.,0.));
#6069=DIRECTION('center_axis',(0.,1.,0.));
#6070=DIRECTION('ref_axis',(1.,0.,0.));
#6071=DIRECTION('',(0.,1.,0.));
#6072=DIRECTION('center_axis',(0.,-1.,0.));
#6073=DIRECTION('ref_axis',(1.,0.,0.));
#6074=DIRECTION('center_axis',(0.,1.,0.));
#6075=DIRECTION('ref_axis',(1.,0.,0.));
#6076=DIRECTION('',(-1.,0.,0.));
#6077=DIRECTION('',(0.,0.,-1.));
#6078=DIRECTION('',(1.,0.,0.));
#6079=DIRECTION('',(0.,0.,1.));
#6080=DIRECTION('center_axis',(0.,1.,0.));
#6081=DIRECTION('ref_axis',(1.,0.,0.));
#6082=DIRECTION('',(-1.,0.,0.));
#6083=DIRECTION('',(0.,0.,1.));
#6084=DIRECTION('',(-1.,0.,0.));
#6085=DIRECTION('',(0.,0.,-1.));
#6086=DIRECTION('center_axis',(0.,0.,-1.));
#6087=DIRECTION('ref_axis',(-1.,0.,0.));
#6088=DIRECTION('',(0.,1.,0.));
#6089=DIRECTION('',(-1.,0.,0.));
#6090=DIRECTION('',(0.,1.,0.));
#6091=DIRECTION('center_axis',(0.,0.,1.));
#6092=DIRECTION('ref_axis',(1.,0.,0.));
#6093=DIRECTION('',(0.,1.,0.));
#6094=DIRECTION('',(1.,0.,0.));
#6095=DIRECTION('',(0.,1.,0.));
#6096=DIRECTION('center_axis',(0.,1.,0.));
#6097=DIRECTION('ref_axis',(0.,0.,1.));
#6098=DIRECTION('',(0.,0.,-1.));
#6099=DIRECTION('',(0.,0.,1.));
#6100=DIRECTION('center_axis',(0.,0.,1.));
#6101=DIRECTION('ref_axis',(1.,0.,0.));
#6102=DIRECTION('center_axis',(0.,0.,1.));
#6103=DIRECTION('ref_axis',(1.,0.,0.));
#6104=DIRECTION('',(0.,0.,1.));
#6105=DIRECTION('center_axis',(0.,0.,-1.));
#6106=DIRECTION('ref_axis',(1.,0.,0.));
#6107=DIRECTION('center_axis',(1.,0.,0.));
#6108=DIRECTION('ref_axis',(0.,1.,0.));
#6109=DIRECTION('',(0.,1.,0.));
#6110=DIRECTION('',(0.,1.,0.));
#6111=DIRECTION('',(0.,0.,1.));
#6112=DIRECTION('center_axis',(0.,-1.,0.));
#6113=DIRECTION('ref_axis',(1.,0.,0.));
#6114=DIRECTION('',(1.,0.,0.));
#6115=DIRECTION('',(1.,0.,0.));
#6116=DIRECTION('',(0.,0.,1.));
#6117=DIRECTION('center_axis',(-1.,0.,0.));
#6118=DIRECTION('ref_axis',(0.,-1.,0.));
#6119=DIRECTION('',(0.,-1.,0.));
#6120=DIRECTION('',(0.,-1.,0.));
#6121=DIRECTION('center_axis',(0.,0.,1.));
#6122=DIRECTION('ref_axis',(1.,0.,0.));
#6123=DIRECTION('center_axis',(0.,0.,1.));
#6124=DIRECTION('ref_axis',(1.,0.,0.));
#6125=DIRECTION('axis',(0.,0.,1.));
#6126=DIRECTION('refdir',(1.,0.,0.));
#6127=DIRECTION('center_axis',(0.,1.,0.));
#6128=DIRECTION('ref_axis',(1.,0.,0.));
#6129=DIRECTION('',(-0.5,0.,0.866025403784439));
#6130=DIRECTION('',(-1.,0.,-3.29650746237182E-16));
#6131=DIRECTION('',(-0.5,0.,-0.866025403784439));
#6132=DIRECTION('',(0.5,0.,-0.866025403784438));
#6133=DIRECTION('',(1.,0.,0.));
#6134=DIRECTION('',(0.5,0.,0.866025403784439));
#6135=DIRECTION('center_axis',(0.,-1.,0.));
#6136=DIRECTION('ref_axis',(1.,0.,0.));
#6137=DIRECTION('center_axis',(0.,1.,0.));
#6138=DIRECTION('ref_axis',(1.,0.,0.));
#6139=DIRECTION('',(0.5,0.,-0.866025403784439));
#6140=DIRECTION('',(-0.5,0.,-0.866025403784439));
#6141=DIRECTION('',(-1.,0.,0.));
#6142=DIRECTION('',(-0.5,0.,0.866025403784438));
#6143=DIRECTION('',(0.5,0.,0.866025403784439));
#6144=DIRECTION('',(1.,0.,3.29650746237182E-16));
#6145=DIRECTION('center_axis',(0.,1.,0.));
#6146=DIRECTION('ref_axis',(1.,0.,0.));
#6147=DIRECTION('center_axis',(-3.29650746237182E-16,0.,1.));
#6148=DIRECTION('ref_axis',(1.,0.,3.29650746237182E-16));
#6149=DIRECTION('',(0.,-1.,0.));
#6150=DIRECTION('',(0.,1.,0.));
#6151=DIRECTION('center_axis',(-0.866025403784439,0.,0.5));
#6152=DIRECTION('ref_axis',(0.5,0.,0.866025403784439));
#6153=DIRECTION('',(0.,1.,0.));
#6154=DIRECTION('center_axis',(-0.866025403784439,0.,-0.5));
#6155=DIRECTION('ref_axis',(-0.5,0.,0.866025403784439));
#6156=DIRECTION('',(0.,1.,0.));
#6157=DIRECTION('center_axis',(0.,0.,-1.));
#6158=DIRECTION('ref_axis',(-1.,0.,0.));
#6159=DIRECTION('',(0.,1.,0.));
#6160=DIRECTION('center_axis',(0.866025403784439,0.,-0.5));
#6161=DIRECTION('ref_axis',(-0.5,0.,-0.866025403784439));
#6162=DIRECTION('',(0.,1.,0.));
#6163=DIRECTION('center_axis',(0.866025403784439,0.,0.5));
#6164=DIRECTION('ref_axis',(0.5,0.,-0.866025403784439));
#6165=DIRECTION('center_axis',(0.,-1.,0.));
#6166=DIRECTION('ref_axis',(1.,0.,0.));
#6167=DIRECTION('',(0.,1.,0.));
#6168=DIRECTION('center_axis',(0.,-1.,0.));
#6169=DIRECTION('ref_axis',(1.,0.,0.));
#6170=DIRECTION('center_axis',(0.,1.,0.));
#6171=DIRECTION('ref_axis',(0.,0.,1.));
#6172=DIRECTION('center_axis',(0.,-1.,0.));
#6173=DIRECTION('ref_axis',(1.,0.,0.));
#6174=DIRECTION('center_axis',(0.,-1.,0.));
#6175=DIRECTION('ref_axis',(1.,0.,0.));
#6176=DIRECTION('center_axis',(0.,-1.,0.));
#6177=DIRECTION('ref_axis',(1.,0.,0.));
#6178=DIRECTION('',(0.707106781186547,0.707106781186548,8.65956056235493E-17));
#6179=DIRECTION('center_axis',(0.,-1.,0.));
#6180=DIRECTION('ref_axis',(1.,0.,0.));
#6181=DIRECTION('center_axis',(0.,-1.,0.));
#6182=DIRECTION('ref_axis',(1.,0.,0.));
#6183=DIRECTION('',(0.,1.,0.));
#6184=DIRECTION('center_axis',(0.,1.,0.));
#6185=DIRECTION('ref_axis',(1.,0.,0.));
#6186=DIRECTION('center_axis',(0.,-1.,0.));
#6187=DIRECTION('ref_axis',(1.,0.,0.));
#6188=DIRECTION('',(-0.707106781186547,0.707106781186548,-8.65956056235493E-17));
#6189=DIRECTION('center_axis',(0.,-1.,0.));
#6190=DIRECTION('ref_axis',(0.,0.,-1.));
#6191=DIRECTION('center_axis',(0.,-1.,0.));
#6192=DIRECTION('ref_axis',(1.,0.,0.));
#6193=DIRECTION('center_axis',(0.,-1.,0.));
#6194=DIRECTION('ref_axis',(1.,0.,0.));
#6195=DIRECTION('',(0.,1.,0.));
#6196=DIRECTION('axis',(0.,0.,1.));
#6197=DIRECTION('refdir',(1.,0.,0.));
#6198=DIRECTION('center_axis',(0.,0.,1.));
#6199=DIRECTION('ref_axis',(1.,0.,0.));
#6200=DIRECTION('center_axis',(0.,0.,-1.));
#6201=DIRECTION('ref_axis',(1.,0.,0.));
#6202=DIRECTION('',(0.,0.,-1.));
#6203=DIRECTION('center_axis',(0.,0.,-1.));
#6204=DIRECTION('ref_axis',(1.,0.,0.));
#6205=DIRECTION('center_axis',(0.,0.,1.));
#6206=DIRECTION('ref_axis',(1.,0.,0.));
#6207=DIRECTION('center_axis',(0.,0.,1.));
#6208=DIRECTION('ref_axis',(1.,0.,0.));
#6209=DIRECTION('',(0.,0.,-1.));
#6210=DIRECTION('center_axis',(0.,0.,1.));
#6211=DIRECTION('ref_axis',(1.,0.,0.));
#6212=DIRECTION('center_axis',(0.,0.,1.));
#6213=DIRECTION('ref_axis',(1.,0.,0.));
#6214=DIRECTION('center_axis',(0.,0.,1.));
#6215=DIRECTION('ref_axis',(1.,0.,0.));
#6216=DIRECTION('axis',(0.,0.,1.));
#6217=DIRECTION('refdir',(1.,0.,0.));
#6218=DIRECTION('center_axis',(0.,0.,1.));
#6219=DIRECTION('ref_axis',(1.,0.,0.));
#6220=DIRECTION('center_axis',(0.,0.,1.));
#6221=DIRECTION('ref_axis',(1.,0.,0.));
#6222=DIRECTION('center_axis',(0.,0.,-1.));
#6223=DIRECTION('ref_axis',(1.,0.,0.));
#6224=DIRECTION('center_axis',(0.,0.,1.));
#6225=DIRECTION('ref_axis',(1.,0.,0.));
#6226=DIRECTION('center_axis',(0.,0.,1.));
#6227=DIRECTION('ref_axis',(1.,0.,0.));
#6228=DIRECTION('',(0.,0.,-1.));
#6229=DIRECTION('center_axis',(0.,0.,1.));
#6230=DIRECTION('ref_axis',(1.,0.,0.));
#6231=DIRECTION('center_axis',(0.,0.,1.));
#6232=DIRECTION('ref_axis',(1.,0.,0.));
#6233=DIRECTION('center_axis',(0.,0.,1.));
#6234=DIRECTION('ref_axis',(1.,0.,0.));
#6235=DIRECTION('center_axis',(0.,0.,1.));
#6236=DIRECTION('ref_axis',(1.,0.,0.));
#6237=DIRECTION('center_axis',(0.,0.,1.));
#6238=DIRECTION('ref_axis',(1.,0.,0.));
#6239=DIRECTION('center_axis',(0.,0.,-1.));
#6240=DIRECTION('ref_axis',(1.,0.,0.));
#6241=DIRECTION('center_axis',(0.,0.,1.));
#6242=DIRECTION('ref_axis',(1.,0.,0.));
#6243=DIRECTION('',(0.,0.,-1.));
#6244=DIRECTION('center_axis',(0.,0.,1.));
#6245=DIRECTION('ref_axis',(1.,0.,0.));
#6246=DIRECTION('',(0.,0.,-1.));
#6247=DIRECTION('center_axis',(0.,0.,-1.));
#6248=DIRECTION('ref_axis',(1.,0.,0.));
#6249=DIRECTION('center_axis',(0.,0.,1.));
#6250=DIRECTION('ref_axis',(1.,0.,0.));
#6251=DIRECTION('',(0.,0.,-1.));
#6252=DIRECTION('center_axis',(0.,0.,1.));
#6253=DIRECTION('ref_axis',(1.,0.,0.));
#6254=DIRECTION('center_axis',(0.,0.,1.));
#6255=DIRECTION('ref_axis',(1.,0.,0.));
#6256=DIRECTION('center_axis',(0.,0.,1.));
#6257=DIRECTION('ref_axis',(1.,0.,0.));
#6258=DIRECTION('',(0.,0.,-1.));
#6259=DIRECTION('center_axis',(0.,0.,1.));
#6260=DIRECTION('ref_axis',(1.,0.,0.));
#6261=DIRECTION('center_axis',(0.,0.,1.));
#6262=DIRECTION('ref_axis',(1.,0.,0.));
#6263=DIRECTION('center_axis',(0.,0.,1.));
#6264=DIRECTION('ref_axis',(1.,0.,0.));
#6265=DIRECTION('axis',(0.,0.,1.));
#6266=DIRECTION('refdir',(1.,0.,0.));
#6267=DIRECTION('center_axis',(0.,0.,1.));
#6268=DIRECTION('ref_axis',(1.,0.,0.));
#6269=DIRECTION('center_axis',(0.,0.,-1.));
#6270=DIRECTION('ref_axis',(1.,0.,0.));
#6271=DIRECTION('',(0.,0.,-1.));
#6272=DIRECTION('center_axis',(0.,0.,-1.));
#6273=DIRECTION('ref_axis',(1.,0.,0.));
#6274=DIRECTION('center_axis',(0.,0.,1.));
#6275=DIRECTION('ref_axis',(1.,0.,0.));
#6276=DIRECTION('center_axis',(0.,0.,1.));
#6277=DIRECTION('ref_axis',(1.,0.,0.));
#6278=DIRECTION('',(0.,0.,-1.));
#6279=DIRECTION('center_axis',(0.,0.,1.));
#6280=DIRECTION('ref_axis',(1.,0.,0.));
#6281=DIRECTION('center_axis',(0.,0.,1.));
#6282=DIRECTION('ref_axis',(1.,0.,0.));
#6283=DIRECTION('center_axis',(0.,0.,1.));
#6284=DIRECTION('ref_axis',(1.,0.,0.));
#6285=DIRECTION('axis',(0.,0.,1.));
#6286=DIRECTION('refdir',(1.,0.,0.));
#6287=DIRECTION('center_axis',(0.,0.,1.));
#6288=DIRECTION('ref_axis',(1.,0.,0.));
#6289=DIRECTION('center_axis',(0.,0.,1.));
#6290=DIRECTION('ref_axis',(1.,0.,0.));
#6291=DIRECTION('',(0.,0.,1.));
#6292=DIRECTION('center_axis',(0.,0.,-1.));
#6293=DIRECTION('ref_axis',(1.,0.,0.));
#6294=DIRECTION('center_axis',(0.,0.,1.));
#6295=DIRECTION('ref_axis',(1.,0.,0.));
#6296=DIRECTION('center_axis',(0.,0.,1.));
#6297=DIRECTION('ref_axis',(1.,0.,0.));
#6298=DIRECTION('',(0.,0.,1.));
#6299=DIRECTION('center_axis',(0.,0.,-1.));
#6300=DIRECTION('ref_axis',(1.,0.,0.));
#6301=DIRECTION('center_axis',(0.,0.,1.));
#6302=DIRECTION('ref_axis',(1.,0.,0.));
#6303=DIRECTION('center_axis',(0.,0.,1.));
#6304=DIRECTION('ref_axis',(1.,0.,0.));
#6305=DIRECTION('',(0.,0.,1.));
#6306=DIRECTION('center_axis',(0.,0.,-1.));
#6307=DIRECTION('ref_axis',(1.,0.,0.));
#6308=DIRECTION('center_axis',(0.,0.,1.));
#6309=DIRECTION('ref_axis',(1.,0.,0.));
#6310=DIRECTION('center_axis',(0.,0.,1.));
#6311=DIRECTION('ref_axis',(1.,0.,0.));
#6312=DIRECTION('',(0.,0.,1.));
#6313=DIRECTION('center_axis',(0.,0.,-1.));
#6314=DIRECTION('ref_axis',(1.,0.,0.));
#6315=DIRECTION('center_axis',(0.,0.,1.));
#6316=DIRECTION('ref_axis',(1.,0.,0.));
#6317=DIRECTION('center_axis',(0.,0.,1.));
#6318=DIRECTION('ref_axis',(1.,0.,0.));
#6319=DIRECTION('',(0.,0.,1.));
#6320=DIRECTION('center_axis',(0.,0.,-1.));
#6321=DIRECTION('ref_axis',(1.,0.,0.));
#6322=DIRECTION('center_axis',(0.,0.,1.));
#6323=DIRECTION('ref_axis',(1.,0.,0.));
#6324=DIRECTION('center_axis',(0.,0.,1.));
#6325=DIRECTION('ref_axis',(1.,0.,0.));
#6326=DIRECTION('',(0.,0.,1.));
#6327=DIRECTION('center_axis',(0.,0.,-1.));
#6328=DIRECTION('ref_axis',(1.,0.,0.));
#6329=DIRECTION('center_axis',(0.,0.,1.));
#6330=DIRECTION('ref_axis',(1.,0.,0.));
#6331=DIRECTION('center_axis',(0.,0.,-1.));
#6332=DIRECTION('ref_axis',(1.,0.,0.));
#6333=DIRECTION('',(0.,0.,-1.));
#6334=DIRECTION('center_axis',(0.,0.,-1.));
#6335=DIRECTION('ref_axis',(1.,0.,0.));
#6336=DIRECTION('center_axis',(0.,0.,1.));
#6337=DIRECTION('ref_axis',(1.,0.,0.));
#6338=DIRECTION('center_axis',(0.,0.,1.));
#6339=DIRECTION('ref_axis',(1.,0.,0.));
#6340=DIRECTION('',(0.,0.,-1.));
#6341=DIRECTION('center_axis',(0.,0.,1.));
#6342=DIRECTION('ref_axis',(1.,0.,0.));
#6343=DIRECTION('center_axis',(0.,0.,1.));
#6344=DIRECTION('ref_axis',(1.,0.,0.));
#6345=DIRECTION('center_axis',(0.,0.,1.));
#6346=DIRECTION('ref_axis',(1.,0.,0.));
#6347=DIRECTION('axis',(0.,0.,1.));
#6348=DIRECTION('refdir',(1.,0.,0.));
#6349=DIRECTION('center_axis',(0.,0.,1.));
#6350=DIRECTION('ref_axis',(1.,0.,0.));
#6351=DIRECTION('center_axis',(0.,0.,-1.));
#6352=DIRECTION('ref_axis',(1.,0.,0.));
#6353=DIRECTION('',(0.,0.,-1.));
#6354=DIRECTION('center_axis',(0.,0.,1.));
#6355=DIRECTION('ref_axis',(1.,0.,0.));
#6356=DIRECTION('center_axis',(0.,0.,1.));
#6357=DIRECTION('ref_axis',(1.,0.,0.));
#6358=DIRECTION('center_axis',(0.,0.,1.));
#6359=DIRECTION('ref_axis',(1.,0.,0.));
#6360=DIRECTION('',(0.,0.,-1.));
#6361=DIRECTION('center_axis',(0.,0.,-1.));
#6362=DIRECTION('ref_axis',(1.,0.,0.));
#6363=DIRECTION('center_axis',(0.,0.,1.));
#6364=DIRECTION('ref_axis',(1.,0.,0.));
#6365=DIRECTION('center_axis',(0.,0.,1.));
#6366=DIRECTION('ref_axis',(1.,0.,0.));
#6367=DIRECTION('center_axis',(0.,0.,1.));
#6368=DIRECTION('ref_axis',(1.,0.,0.));
#6369=DIRECTION('center_axis',(0.,0.,1.));
#6370=DIRECTION('ref_axis',(1.,0.,0.));
#6371=DIRECTION('center_axis',(0.,0.,-1.));
#6372=DIRECTION('ref_axis',(1.,0.,0.));
#6373=DIRECTION('',(0.,0.,-1.));
#6374=DIRECTION('center_axis',(0.,0.,-1.));
#6375=DIRECTION('ref_axis',(1.,0.,0.));
#6376=DIRECTION('center_axis',(0.,0.,1.));
#6377=DIRECTION('ref_axis',(1.,0.,0.));
#6378=DIRECTION('',(0.,0.,-1.));
#6379=DIRECTION('center_axis',(0.,0.,1.));
#6380=DIRECTION('ref_axis',(1.,0.,0.));
#6381=DIRECTION('center_axis',(0.,0.,1.));
#6382=DIRECTION('ref_axis',(1.,0.,0.));
#6383=DIRECTION('center_axis',(0.,0.,1.));
#6384=DIRECTION('ref_axis',(1.,0.,0.));
#6385=DIRECTION('axis',(0.,0.,1.));
#6386=DIRECTION('refdir',(1.,0.,0.));
#6387=DIRECTION('center_axis',(0.,0.,1.));
#6388=DIRECTION('ref_axis',(1.,0.,0.));
#6389=DIRECTION('center_axis',(0.,0.,1.));
#6390=DIRECTION('ref_axis',(1.,0.,0.));
#6391=DIRECTION('center_axis',(0.,0.,1.));
#6392=DIRECTION('ref_axis',(1.,0.,0.));
#6393=DIRECTION('center_axis',(0.,0.,1.));
#6394=DIRECTION('ref_axis',(1.,0.,0.));
#6395=DIRECTION('',(0.,0.,1.));
#6396=DIRECTION('center_axis',(0.,0.,1.));
#6397=DIRECTION('ref_axis',(1.,0.,0.));
#6398=DIRECTION('',(0.,0.,-1.));
#6399=DIRECTION('center_axis',(0.,0.,1.));
#6400=DIRECTION('ref_axis',(-0.866025403784439,-0.5,0.));
#6401=DIRECTION('',(0.,0.,-1.));
#6402=DIRECTION('center_axis',(0.,0.,1.));
#6403=DIRECTION('ref_axis',(1.,0.,0.));
#6404=DIRECTION('',(0.,0.,1.));
#6405=DIRECTION('center_axis',(0.,0.,1.));
#6406=DIRECTION('ref_axis',(1.,0.,0.));
#6407=DIRECTION('center_axis',(0.,0.,1.));
#6408=DIRECTION('ref_axis',(1.,0.,0.));
#6409=DIRECTION('center_axis',(0.,0.,1.));
#6410=DIRECTION('ref_axis',(1.,0.,0.));
#6411=DIRECTION('center_axis',(0.,0.,1.));
#6412=DIRECTION('ref_axis',(1.,0.,0.));
#6413=DIRECTION('center_axis',(0.,0.,1.));
#6414=DIRECTION('ref_axis',(1.,0.,0.));
#6415=DIRECTION('center_axis',(0.,0.,1.));
#6416=DIRECTION('ref_axis',(1.,0.,0.));
#6417=DIRECTION('center_axis',(0.,0.,1.));
#6418=DIRECTION('ref_axis',(1.,0.,0.));
#6419=DIRECTION('',(0.,0.,1.));
#6420=DIRECTION('center_axis',(0.,0.,1.));
#6421=DIRECTION('ref_axis',(1.,0.,0.));
#6422=DIRECTION('',(0.,0.,-1.));
#6423=DIRECTION('center_axis',(0.,0.,1.));
#6424=DIRECTION('ref_axis',(1.,0.,0.));
#6425=DIRECTION('center_axis',(0.,0.,1.));
#6426=DIRECTION('ref_axis',(1.,0.,0.));
#6427=DIRECTION('center_axis',(0.,0.,1.));
#6428=DIRECTION('ref_axis',(1.,0.,0.));
#6429=DIRECTION('center_axis',(0.,0.,1.));
#6430=DIRECTION('ref_axis',(1.,0.,0.));
#6431=DIRECTION('',(0.,0.,1.));
#6432=DIRECTION('center_axis',(0.,0.,1.));
#6433=DIRECTION('ref_axis',(1.,0.,0.));
#6434=DIRECTION('',(0.,0.,-1.));
#6435=DIRECTION('center_axis',(0.,0.,1.));
#6436=DIRECTION('ref_axis',(1.,0.,0.));
#6437=DIRECTION('center_axis',(0.,0.,1.));
#6438=DIRECTION('ref_axis',(1.,0.,0.));
#6439=DIRECTION('center_axis',(0.,0.,1.));
#6440=DIRECTION('ref_axis',(1.,0.,0.));
#6441=DIRECTION('center_axis',(0.,0.,1.));
#6442=DIRECTION('ref_axis',(1.,0.,0.));
#6443=DIRECTION('',(0.,0.,1.));
#6444=DIRECTION('center_axis',(0.,0.,1.));
#6445=DIRECTION('ref_axis',(1.,0.,0.));
#6446=DIRECTION('',(0.,0.,-1.));
#6447=DIRECTION('center_axis',(0.,0.,1.));
#6448=DIRECTION('ref_axis',(-0.866025403784438,0.5,0.));
#6449=DIRECTION('',(0.,0.,-1.));
#6450=DIRECTION('center_axis',(0.,0.,1.));
#6451=DIRECTION('ref_axis',(1.,0.,0.));
#6452=DIRECTION('',(0.,0.,1.));
#6453=DIRECTION('center_axis',(0.,0.,1.));
#6454=DIRECTION('ref_axis',(1.,0.,0.));
#6455=DIRECTION('center_axis',(0.,0.,1.));
#6456=DIRECTION('ref_axis',(1.,0.,0.));
#6457=DIRECTION('center_axis',(0.,0.,1.));
#6458=DIRECTION('ref_axis',(1.,0.,0.));
#6459=DIRECTION('center_axis',(0.,0.,1.));
#6460=DIRECTION('ref_axis',(1.,0.,0.));
#6461=DIRECTION('center_axis',(0.,0.,1.));
#6462=DIRECTION('ref_axis',(1.,0.,0.));
#6463=DIRECTION('',(0.,0.,-1.));
#6464=DIRECTION('center_axis',(0.,0.,-1.));
#6465=DIRECTION('ref_axis',(1.,0.,0.));
#6466=DIRECTION('center_axis',(0.,0.,-1.));
#6467=DIRECTION('ref_axis',(1.,0.,0.));
#6468=DIRECTION('center_axis',(0.,0.,-1.));
#6469=DIRECTION('ref_axis',(1.,0.,0.));
#6470=DIRECTION('center_axis',(0.,0.,-1.));
#6471=DIRECTION('ref_axis',(1.,0.,0.));
#6472=DIRECTION('center_axis',(0.,0.,-1.));
#6473=DIRECTION('ref_axis',(1.,0.,0.));
#6474=DIRECTION('center_axis',(0.,0.,-1.));
#6475=DIRECTION('ref_axis',(1.,0.,0.));
#6476=DIRECTION('center_axis',(0.,0.,-1.));
#6477=DIRECTION('ref_axis',(1.,0.,0.));
#6478=DIRECTION('center_axis',(0.,0.,1.));
#6479=DIRECTION('ref_axis',(1.,0.,0.));
#6480=DIRECTION('center_axis',(0.,0.,1.));
#6481=DIRECTION('ref_axis',(1.,0.,0.));
#6482=DIRECTION('',(0.,0.,1.));
#6483=DIRECTION('center_axis',(0.,0.,-1.));
#6484=DIRECTION('ref_axis',(1.,0.,0.));
#6485=DIRECTION('center_axis',(0.,0.,1.));
#6486=DIRECTION('ref_axis',(1.,0.,0.));
#6487=DIRECTION('center_axis',(0.,0.,1.));
#6488=DIRECTION('ref_axis',(1.,0.,0.));
#6489=DIRECTION('',(0.,0.,1.));
#6490=DIRECTION('center_axis',(0.,0.,-1.));
#6491=DIRECTION('ref_axis',(1.,0.,0.));
#6492=DIRECTION('center_axis',(0.,0.,1.));
#6493=DIRECTION('ref_axis',(1.,0.,0.));
#6494=DIRECTION('center_axis',(0.,0.,1.));
#6495=DIRECTION('ref_axis',(1.,0.,0.));
#6496=DIRECTION('',(0.,0.,1.));
#6497=DIRECTION('center_axis',(0.,0.,-1.));
#6498=DIRECTION('ref_axis',(1.,0.,0.));
#6499=DIRECTION('center_axis',(0.,0.,1.));
#6500=DIRECTION('ref_axis',(1.,0.,0.));
#6501=DIRECTION('center_axis',(0.,0.,1.));
#6502=DIRECTION('ref_axis',(1.,0.,0.));
#6503=DIRECTION('',(0.,0.,1.));
#6504=DIRECTION('center_axis',(0.,0.,-1.));
#6505=DIRECTION('ref_axis',(1.,0.,0.));
#6506=DIRECTION('center_axis',(0.,0.,1.));
#6507=DIRECTION('ref_axis',(1.,0.,0.));
#6508=DIRECTION('center_axis',(0.,0.,1.));
#6509=DIRECTION('ref_axis',(1.,0.,0.));
#6510=DIRECTION('',(0.,0.,1.));
#6511=DIRECTION('center_axis',(0.,0.,-1.));
#6512=DIRECTION('ref_axis',(1.,0.,0.));
#6513=DIRECTION('center_axis',(0.,0.,1.));
#6514=DIRECTION('ref_axis',(1.,0.,0.));
#6515=DIRECTION('center_axis',(0.,0.,1.));
#6516=DIRECTION('ref_axis',(1.,0.,0.));
#6517=DIRECTION('',(0.,0.,1.));
#6518=DIRECTION('center_axis',(0.,0.,-1.));
#6519=DIRECTION('ref_axis',(1.,0.,0.));
#6520=DIRECTION('center_axis',(0.,0.,1.));
#6521=DIRECTION('ref_axis',(1.,0.,0.));
#6522=DIRECTION('center_axis',(0.,0.,1.));
#6523=DIRECTION('ref_axis',(1.,0.,0.));
#6524=DIRECTION('',(0.,0.,1.));
#6525=DIRECTION('center_axis',(0.,0.,-1.));
#6526=DIRECTION('ref_axis',(1.,0.,0.));
#6527=DIRECTION('center_axis',(0.,0.,1.));
#6528=DIRECTION('ref_axis',(1.,0.,0.));
#6529=DIRECTION('center_axis',(0.,0.,1.));
#6530=DIRECTION('ref_axis',(1.,0.,0.));
#6531=DIRECTION('',(0.,0.,1.));
#6532=DIRECTION('center_axis',(0.,0.,1.));
#6533=DIRECTION('ref_axis',(1.,0.,0.));
#6534=DIRECTION('center_axis',(0.,0.,1.));
#6535=DIRECTION('ref_axis',(1.,0.,0.));
#6536=DIRECTION('center_axis',(0.,0.,1.));
#6537=DIRECTION('ref_axis',(1.,0.,0.));
#6538=DIRECTION('center_axis',(0.,0.,1.));
#6539=DIRECTION('ref_axis',(1.,0.,0.));
#6540=DIRECTION('center_axis',(0.,0.,1.));
#6541=DIRECTION('ref_axis',(1.,0.,0.));
#6542=DIRECTION('',(0.,0.,-1.));
#6543=DIRECTION('center_axis',(0.,0.,1.));
#6544=DIRECTION('ref_axis',(1.,0.,0.));
#6545=DIRECTION('center_axis',(0.,0.,1.));
#6546=DIRECTION('ref_axis',(1.,0.,0.));
#6547=DIRECTION('center_axis',(0.,0.,1.));
#6548=DIRECTION('ref_axis',(1.,0.,0.));
#6549=DIRECTION('axis',(0.,0.,1.));
#6550=DIRECTION('refdir',(1.,0.,0.));
#6551=DIRECTION('center_axis',(-0.000134591856444243,0.997598919682403,
0.0692558830247305));
#6552=DIRECTION('ref_axis',(9.34371278597603E-6,-0.0692558823944232,0.997598928761687));
#6553=DIRECTION('center_axis',(0.000134591670588553,0.997598919668532,0.0692558832248945));
#6554=DIRECTION('ref_axis',(-0.499431472094232,0.0600671278230296,-0.864268560597272));
#6555=DIRECTION('center_axis',(0.000134591670588553,0.997598919668532,0.0692558832248945));
#6556=DIRECTION('ref_axis',(-0.499431472094232,0.0600671278230296,-0.864268560597272));
#6557=DIRECTION('center_axis',(-0.000134591856444243,0.997598919682403,
0.0692558830247305));
#6558=DIRECTION('ref_axis',(9.34371278597603E-6,-0.0692558823944232,0.997598928761687));
#6559=DIRECTION('axis',(0.,0.,1.));
#6560=DIRECTION('refdir',(1.,0.,0.));
#6561=DIRECTION('center_axis',(0.,0.,1.));
#6562=DIRECTION('ref_axis',(1.,0.,0.));
#6563=DIRECTION('center_axis',(0.,0.,1.));
#6564=DIRECTION('ref_axis',(1.,0.,0.));
#6565=DIRECTION('',(0.,0.,-1.));
#6566=DIRECTION('center_axis',(0.,0.,1.));
#6567=DIRECTION('ref_axis',(1.,0.,0.));
#6568=DIRECTION('center_axis',(0.,0.,1.));
#6569=DIRECTION('ref_axis',(1.,0.,0.));
#6570=DIRECTION('center_axis',(0.,0.,1.));
#6571=DIRECTION('ref_axis',(1.,0.,0.));
#6572=DIRECTION('center_axis',(0.,0.,1.));
#6573=DIRECTION('ref_axis',(1.,0.,0.));
#6574=DIRECTION('',(0.,0.,-1.));
#6575=DIRECTION('center_axis',(0.,0.,1.));
#6576=DIRECTION('ref_axis',(1.,0.,0.));
#6577=DIRECTION('center_axis',(0.,0.,1.));
#6578=DIRECTION('ref_axis',(1.,0.,0.));
#6579=DIRECTION('center_axis',(0.,0.,1.));
#6580=DIRECTION('ref_axis',(1.,0.,0.));
#6581=DIRECTION('axis',(0.,0.,1.));
#6582=DIRECTION('refdir',(1.,0.,0.));
#6583=DIRECTION('center_axis',(0.,0.,1.));
#6584=DIRECTION('ref_axis',(1.,0.,0.));
#6585=DIRECTION('center_axis',(0.,0.,1.));
#6586=DIRECTION('ref_axis',(1.,0.,0.));
#6587=DIRECTION('',(0.,0.,-1.));
#6588=DIRECTION('center_axis',(0.,0.,1.));
#6589=DIRECTION('ref_axis',(1.,0.,0.));
#6590=DIRECTION('center_axis',(0.,0.,1.));
#6591=DIRECTION('ref_axis',(1.,0.,0.));
#6592=DIRECTION('center_axis',(0.,0.,1.));
#6593=DIRECTION('ref_axis',(1.,0.,0.));
#6594=DIRECTION('axis',(0.,0.,1.));
#6595=DIRECTION('refdir',(1.,0.,0.));
#6596=DIRECTION('center_axis',(0.,1.,0.));
#6597=DIRECTION('ref_axis',(1.,0.,0.));
#6598=DIRECTION('',(0.,0.,1.));
#6599=DIRECTION('center_axis',(0.,1.,0.));
#6600=DIRECTION('ref_axis',(1.,0.,0.));
#6601=DIRECTION('center_axis',(0.,1.,0.));
#6602=DIRECTION('ref_axis',(1.,0.,0.));
#6603=DIRECTION('center_axis',(0.,1.,0.));
#6604=DIRECTION('ref_axis',(1.,0.,0.));
#6605=DIRECTION('center_axis',(0.,1.,0.));
#6606=DIRECTION('ref_axis',(1.,0.,0.));
#6607=DIRECTION('',(0.,1.,0.));
#6608=DIRECTION('center_axis',(0.,1.,0.));
#6609=DIRECTION('ref_axis',(1.,0.,0.));
#6610=DIRECTION('',(0.,0.,-1.));
#6611=DIRECTION('center_axis',(0.,0.,1.));
#6612=DIRECTION('ref_axis',(1.,0.,0.));
#6613=DIRECTION('center_axis',(0.,0.,-1.));
#6614=DIRECTION('ref_axis',(1.,0.,0.));
#6615=DIRECTION('',(0.,0.,-1.));
#6616=DIRECTION('center_axis',(0.,0.,-1.));
#6617=DIRECTION('ref_axis',(1.,0.,0.));
#6618=DIRECTION('center_axis',(0.,0.,1.));
#6619=DIRECTION('ref_axis',(1.,0.,0.));
#6620=DIRECTION('center_axis',(0.,0.,1.));
#6621=DIRECTION('ref_axis',(1.,0.,0.));
#6622=DIRECTION('',(0.,0.,-1.));
#6623=DIRECTION('center_axis',(0.,0.,1.));
#6624=DIRECTION('ref_axis',(1.,0.,0.));
#6625=DIRECTION('center_axis',(0.,0.,1.));
#6626=DIRECTION('ref_axis',(1.,0.,0.));
#6627=DIRECTION('center_axis',(0.,0.,1.));
#6628=DIRECTION('ref_axis',(1.,0.,0.));
#6629=DIRECTION('axis',(0.,0.,1.));
#6630=DIRECTION('refdir',(1.,0.,0.));
#6631=DIRECTION('center_axis',(0.,1.,0.));
#6632=DIRECTION('ref_axis',(0.,0.,1.));
#6633=DIRECTION('center_axis',(0.,-1.,0.));
#6634=DIRECTION('ref_axis',(1.,0.,0.));
#6635=DIRECTION('center_axis',(0.,-1.,0.));
#6636=DIRECTION('ref_axis',(1.,0.,0.));
#6637=DIRECTION('center_axis',(0.,-1.,0.));
#6638=DIRECTION('ref_axis',(1.,0.,0.));
#6639=DIRECTION('',(0.707106781186548,0.707106781186547,8.65956056235493E-17));
#6640=DIRECTION('center_axis',(0.,-1.,0.));
#6641=DIRECTION('ref_axis',(1.,0.,0.));
#6642=DIRECTION('center_axis',(0.,-1.,0.));
#6643=DIRECTION('ref_axis',(1.,0.,0.));
#6644=DIRECTION('',(0.,1.,0.));
#6645=DIRECTION('center_axis',(0.,1.,0.));
#6646=DIRECTION('ref_axis',(1.,0.,0.));
#6647=DIRECTION('center_axis',(0.,-1.,0.));
#6648=DIRECTION('ref_axis',(1.,0.,0.));
#6649=DIRECTION('',(-0.707106781186547,0.707106781186548,-8.65956056235493E-17));
#6650=DIRECTION('center_axis',(0.,-1.,0.));
#6651=DIRECTION('ref_axis',(0.,0.,-1.));
#6652=DIRECTION('center_axis',(0.,-1.,0.));
#6653=DIRECTION('ref_axis',(1.,0.,0.));
#6654=DIRECTION('center_axis',(0.,1.,0.));
#6655=DIRECTION('ref_axis',(1.,0.,0.));
#6656=DIRECTION('center_axis',(0.,1.,0.));
#6657=DIRECTION('ref_axis',(1.,0.,0.));
#6658=DIRECTION('',(-0.447213595499958,0.894427190999916,-5.47678698264203E-17));
#6659=DIRECTION('center_axis',(0.,-1.,0.));
#6660=DIRECTION('ref_axis',(1.,0.,0.));
#6661=DIRECTION('center_axis',(0.,1.,0.));
#6662=DIRECTION('ref_axis',(1.,0.,0.));
#6663=DIRECTION('',(0.,1.,0.));
#6664=DIRECTION('center_axis',(0.,1.,0.));
#6665=DIRECTION('ref_axis',(1.,0.,0.));
#6666=DIRECTION('center_axis',(0.,-1.,0.));
#6667=DIRECTION('ref_axis',(1.,0.,0.));
#6668=DIRECTION('',(-0.707106781186547,0.707106781186548,-8.65956056235493E-17));
#6669=DIRECTION('center_axis',(0.,-1.,0.));
#6670=DIRECTION('ref_axis',(0.,0.,-1.));
#6671=DIRECTION('center_axis',(0.866025403784439,0.,-0.5));
#6672=DIRECTION('ref_axis',(0.5,0.,0.866025403784439));
#6673=DIRECTION('',(-0.5,0.,-0.866025403784439));
#6674=DIRECTION('',(0.,-1.,0.));
#6675=DIRECTION('',(0.5,0.,0.866025403784439));
#6676=DIRECTION('',(0.,-1.,0.));
#6677=DIRECTION('center_axis',(1.20185167898973E-16,0.,-1.));
#6678=DIRECTION('ref_axis',(1.,0.,1.20185167898973E-16));
#6679=DIRECTION('',(-1.,0.,-1.20185167898973E-16));
#6680=DIRECTION('',(0.,-1.,0.));
#6681=DIRECTION('',(1.,0.,1.20185167898973E-16));
#6682=DIRECTION('center_axis',(-0.866025403784439,0.,-0.5));
#6683=DIRECTION('ref_axis',(0.5,0.,-0.866025403784439));
#6684=DIRECTION('',(-0.5,0.,0.866025403784439));
#6685=DIRECTION('',(0.,-1.,0.));
#6686=DIRECTION('',(0.5,0.,-0.866025403784439));
#6687=DIRECTION('center_axis',(-0.866025403784439,0.,0.5));
#6688=DIRECTION('ref_axis',(-0.5,0.,-0.866025403784439));
#6689=DIRECTION('',(0.5,0.,0.866025403784439));
#6690=DIRECTION('',(0.,-1.,0.));
#6691=DIRECTION('',(-0.5,0.,-0.866025403784439));
#6692=DIRECTION('center_axis',(-2.40370335797945E-16,0.,1.));
#6693=DIRECTION('ref_axis',(-1.,0.,-2.40370335797945E-16));
#6694=DIRECTION('',(1.,0.,2.40370335797945E-16));
#6695=DIRECTION('',(0.,-1.,0.));
#6696=DIRECTION('',(-1.,0.,-2.40370335797945E-16));
#6697=DIRECTION('center_axis',(0.866025403784439,0.,0.5));
#6698=DIRECTION('ref_axis',(-0.5,0.,0.866025403784439));
#6699=DIRECTION('',(0.5,0.,-0.866025403784439));
#6700=DIRECTION('',(-0.5,0.,0.866025403784439));
#6701=DIRECTION('center_axis',(0.,1.,0.));
#6702=DIRECTION('ref_axis',(1.,0.,0.));
#6703=DIRECTION('center_axis',(0.,-1.,0.));
#6704=DIRECTION('ref_axis',(0.,0.,-1.));
#6705=DIRECTION('axis',(0.,0.,1.));
#6706=DIRECTION('refdir',(1.,0.,0.));
#6707=DIRECTION('center_axis',(0.,1.,0.));
#6708=DIRECTION('ref_axis',(1.,0.,0.));
#6709=DIRECTION('center_axis',(0.,-1.,0.));
#6710=DIRECTION('ref_axis',(1.,0.,0.));
#6711=DIRECTION('',(0.,-1.,0.));
#6712=DIRECTION('center_axis',(0.,-1.,0.));
#6713=DIRECTION('ref_axis',(1.,0.,0.));
#6714=DIRECTION('center_axis',(0.,1.,0.));
#6715=DIRECTION('ref_axis',(1.,0.,0.));
#6716=DIRECTION('center_axis',(0.,1.,0.));
#6717=DIRECTION('ref_axis',(1.,0.,0.));
#6718=DIRECTION('',(0.,-1.,0.));
#6719=DIRECTION('center_axis',(0.,1.,0.));
#6720=DIRECTION('ref_axis',(1.,0.,0.));
#6721=DIRECTION('center_axis',(0.,1.,0.));
#6722=DIRECTION('ref_axis',(1.,0.,0.));
#6723=DIRECTION('center_axis',(0.,1.,0.));
#6724=DIRECTION('ref_axis',(1.,0.,0.));
#6725=DIRECTION('axis',(0.,0.,1.));
#6726=DIRECTION('refdir',(1.,0.,0.));
#6727=DIRECTION('center_axis',(0.,1.,0.));
#6728=DIRECTION('ref_axis',(1.,0.,0.));
#6729=DIRECTION('',(0.866025403784439,-0.5,1.06057523872491E-16));
#6730=DIRECTION('center_axis',(0.,-1.,0.));
#6731=DIRECTION('ref_axis',(1.,0.,0.));
#6732=DIRECTION('center_axis',(0.,-1.,0.));
#6733=DIRECTION('ref_axis',(1.,0.,0.));
#6734=DIRECTION('center_axis',(0.,1.,0.));
#6735=DIRECTION('ref_axis',(1.,0.,0.));
#6736=DIRECTION('',(-0.866025403784439,-0.5,-1.06057523872491E-16));
#6737=DIRECTION('center_axis',(1.4792020664489E-16,0.,-1.));
#6738=DIRECTION('ref_axis',(-1.,0.,-1.4792020664489E-16));
#6739=DIRECTION('',(0.,1.,0.));
#6740=DIRECTION('',(0.,1.,0.));
#6741=DIRECTION('center_axis',(-0.866025403784439,0.,-0.5));
#6742=DIRECTION('ref_axis',(-0.5,0.,0.866025403784439));
#6743=DIRECTION('',(0.,1.,0.));
#6744=DIRECTION('center_axis',(-0.866025403784439,0.,0.5));
#6745=DIRECTION('ref_axis',(0.5,0.,0.866025403784439));
#6746=DIRECTION('',(0.,1.,0.));
#6747=DIRECTION('center_axis',(0.,1.,0.));
#6748=DIRECTION('ref_axis',(1.,0.,0.));
#6749=DIRECTION('center_axis',(0.,1.,0.));
#6750=DIRECTION('ref_axis',(1.,0.,0.));
#6751=DIRECTION('',(0.,-1.,0.));
#6752=DIRECTION('center_axis',(0.,1.,0.));
#6753=DIRECTION('ref_axis',(1.,0.,0.));
#6754=DIRECTION('center_axis',(-2.95840413289779E-16,0.,1.));
#6755=DIRECTION('ref_axis',(1.,0.,2.95840413289779E-16));
#6756=DIRECTION('',(0.,1.,0.));
#6757=DIRECTION('center_axis',(0.866025403784439,0.,-0.5));
#6758=DIRECTION('ref_axis',(-0.5,0.,-0.866025403784439));
#6759=DIRECTION('',(0.,1.,0.));
#6760=DIRECTION('center_axis',(0.866025403784439,0.,0.5));
#6761=DIRECTION('ref_axis',(0.5,0.,-0.866025403784439));
#6762=DIRECTION('center_axis',(0.,1.,0.));
#6763=DIRECTION('ref_axis',(1.,0.,0.));
#6764=DIRECTION('center_axis',(0.,1.,0.));
#6765=DIRECTION('ref_axis',(1.,0.,0.));
#6766=DIRECTION('axis',(0.,0.,1.));
#6767=DIRECTION('refdir',(1.,0.,0.));
#6768=DIRECTION('center_axis',(0.866025403784439,0.,-0.5));
#6769=DIRECTION('ref_axis',(0.5,0.,0.866025403784439));
#6770=DIRECTION('',(0.5,0.,0.866025403784439));
#6771=DIRECTION('',(0.,-1.,0.));
#6772=DIRECTION('',(0.5,0.,0.866025403784439));
#6773=DIRECTION('',(0.,-1.,0.));
#6774=DIRECTION('center_axis',(1.20185167898973E-16,0.,-1.));
#6775=DIRECTION('ref_axis',(1.,0.,1.20185167898973E-16));
#6776=DIRECTION('',(1.,0.,1.20185167898973E-16));
#6777=DIRECTION('',(0.,-1.,0.));
#6778=DIRECTION('',(1.,0.,1.20185167898973E-16));
#6779=DIRECTION('center_axis',(-0.866025403784439,0.,-0.5));
#6780=DIRECTION('ref_axis',(0.5,0.,-0.866025403784439));
#6781=DIRECTION('',(0.5,0.,-0.866025403784439));
#6782=DIRECTION('',(0.,-1.,0.));
#6783=DIRECTION('',(0.5,0.,-0.866025403784439));
#6784=DIRECTION('center_axis',(-0.866025403784439,0.,0.5));
#6785=DIRECTION('ref_axis',(-0.5,0.,-0.866025403784439));
#6786=DIRECTION('',(-0.5,0.,-0.866025403784439));
#6787=DIRECTION('',(0.,-1.,0.));
#6788=DIRECTION('',(-0.5,0.,-0.866025403784439));
#6789=DIRECTION('center_axis',(-2.40370335797945E-16,0.,1.));
#6790=DIRECTION('ref_axis',(-1.,0.,-2.40370335797945E-16));
#6791=DIRECTION('',(-1.,0.,-2.40370335797945E-16));
#6792=DIRECTION('',(0.,-1.,0.));
#6793=DIRECTION('',(-1.,0.,-2.40370335797945E-16));
#6794=DIRECTION('center_axis',(0.866025403784439,0.,0.5));
#6795=DIRECTION('ref_axis',(-0.5,0.,0.866025403784439));
#6796=DIRECTION('',(-0.5,0.,0.866025403784439));
#6797=DIRECTION('',(-0.5,0.,0.866025403784439));
#6798=DIRECTION('center_axis',(0.,-1.,0.));
#6799=DIRECTION('ref_axis',(0.,0.,-1.));
#6800=DIRECTION('center_axis',(0.,1.,0.));
#6801=DIRECTION('ref_axis',(0.,0.,1.));
#6802=DIRECTION('center_axis',(0.,-1.,0.));
#6803=DIRECTION('ref_axis',(1.,0.,0.));
#6804=DIRECTION('center_axis',(0.,-1.,0.));
#6805=DIRECTION('ref_axis',(1.,0.,0.));
#6806=DIRECTION('center_axis',(0.,-1.,0.));
#6807=DIRECTION('ref_axis',(1.,0.,0.));
#6808=DIRECTION('',(0.707106781186548,0.707106781186547,8.65956056235494E-17));
#6809=DIRECTION('center_axis',(0.,-1.,0.));
#6810=DIRECTION('ref_axis',(1.,0.,0.));
#6811=DIRECTION('center_axis',(0.,1.,0.));
#6812=DIRECTION('ref_axis',(1.,0.,0.));
#6813=DIRECTION('',(0.,1.,0.));
#6814=DIRECTION('center_axis',(0.,1.,0.));
#6815=DIRECTION('ref_axis',(1.,0.,0.));
#6816=DIRECTION('center_axis',(0.,-1.,0.));
#6817=DIRECTION('ref_axis',(1.,0.,0.));
#6818=DIRECTION('',(-0.707106781186548,0.707106781186547,-8.65956056235494E-17));
#6819=DIRECTION('center_axis',(0.,-1.,0.));
#6820=DIRECTION('ref_axis',(0.,0.,-1.));
#6821=DIRECTION('axis',(0.,0.,1.));
#6822=DIRECTION('refdir',(1.,0.,0.));
#6823=DIRECTION('center_axis',(0.,-1.,0.));
#6824=DIRECTION('ref_axis',(0.,0.,-1.));
#6825=DIRECTION('center_axis',(-1.,0.,-1.22464679914735E-16));
#6826=DIRECTION('ref_axis',(-1.22464679914735E-16,0.,1.));
#6827=DIRECTION('center_axis',(0.,1.,0.));
#6828=DIRECTION('ref_axis',(0.,0.,-1.));
#6829=DIRECTION('axis',(0.,0.,1.));
#6830=DIRECTION('refdir',(1.,0.,0.));
#6831=DIRECTION('center_axis',(0.,0.,1.));
#6832=DIRECTION('ref_axis',(1.,0.,0.));
#6833=DIRECTION('center_axis',(0.,0.,1.));
#6834=DIRECTION('ref_axis',(1.,0.,0.));
#6835=DIRECTION('',(0.,0.,1.));
#6836=DIRECTION('center_axis',(0.,0.,-1.));
#6837=DIRECTION('ref_axis',(1.,0.,0.));
#6838=DIRECTION('center_axis',(0.,1.,0.));
#6839=DIRECTION('ref_axis',(-1.,0.,0.));
#6840=DIRECTION('',(-1.,0.,0.));
#6841=DIRECTION('',(0.,0.,1.));
#6842=DIRECTION('',(-1.,0.,0.));
#6843=DIRECTION('',(0.,0.,1.));
#6844=DIRECTION('center_axis',(1.,0.,0.));
#6845=DIRECTION('ref_axis',(0.,1.,0.));
#6846=DIRECTION('',(0.,1.,0.));
#6847=DIRECTION('',(0.,1.,0.));
#6848=DIRECTION('',(0.,0.,1.));
#6849=DIRECTION('center_axis',(0.,-1.,0.));
#6850=DIRECTION('ref_axis',(1.,0.,0.));
#6851=DIRECTION('',(1.,0.,0.));
#6852=DIRECTION('',(1.,0.,0.));
#6853=DIRECTION('',(0.,0.,1.));
#6854=DIRECTION('center_axis',(-1.,0.,0.));
#6855=DIRECTION('ref_axis',(0.,-1.,0.));
#6856=DIRECTION('',(0.,-1.,0.));
#6857=DIRECTION('',(0.,-1.,0.));
#6858=DIRECTION('center_axis',(0.,0.,1.));
#6859=DIRECTION('ref_axis',(1.,0.,0.));
#6860=DIRECTION('center_axis',(0.,0.,1.));
#6861=DIRECTION('ref_axis',(1.,0.,0.));
#6862=DIRECTION('axis',(0.,0.,1.));
#6863=DIRECTION('refdir',(1.,0.,0.));
#6864=DIRECTION('center_axis',(0.,1.,0.));
#6865=DIRECTION('ref_axis',(0.,0.,1.));
#6866=DIRECTION('center_axis',(0.,-1.,0.));
#6867=DIRECTION('ref_axis',(1.,0.,0.));
#6868=DIRECTION('center_axis',(0.,-1.,0.));
#6869=DIRECTION('ref_axis',(1.,0.,0.));
#6870=DIRECTION('center_axis',(0.,-1.,0.));
#6871=DIRECTION('ref_axis',(1.,0.,0.));
#6872=DIRECTION('',(0.707106781186547,0.707106781186548,8.65956056235493E-17));
#6873=DIRECTION('center_axis',(0.,-1.,0.));
#6874=DIRECTION('ref_axis',(1.,0.,0.));
#6875=DIRECTION('center_axis',(0.,-1.,0.));
#6876=DIRECTION('ref_axis',(1.,0.,0.));
#6877=DIRECTION('',(0.,1.,0.));
#6878=DIRECTION('center_axis',(0.,1.,0.));
#6879=DIRECTION('ref_axis',(1.,0.,0.));
#6880=DIRECTION('center_axis',(0.,-1.,0.));
#6881=DIRECTION('ref_axis',(1.,0.,0.));
#6882=DIRECTION('',(-0.707106781186547,0.707106781186548,-8.65956056235493E-17));
#6883=DIRECTION('center_axis',(0.,-1.,0.));
#6884=DIRECTION('ref_axis',(0.,0.,-1.));
#6885=DIRECTION('center_axis',(0.,-1.,0.));
#6886=DIRECTION('ref_axis',(1.,0.,0.));
#6887=DIRECTION('center_axis',(0.,1.,0.));
#6888=DIRECTION('ref_axis',(1.,0.,0.));
#6889=DIRECTION('center_axis',(0.,1.,0.));
#6890=DIRECTION('ref_axis',(1.,0.,0.));
#6891=DIRECTION('',(-0.447213595499958,0.894427190999916,-5.47678698264203E-17));
#6892=DIRECTION('center_axis',(0.,-1.,0.));
#6893=DIRECTION('ref_axis',(1.,0.,0.));
#6894=DIRECTION('center_axis',(0.,1.,0.));
#6895=DIRECTION('ref_axis',(1.,0.,0.));
#6896=DIRECTION('',(0.,1.,0.));
#6897=DIRECTION('center_axis',(0.,1.,0.));
#6898=DIRECTION('ref_axis',(1.,0.,0.));
#6899=DIRECTION('center_axis',(0.,-1.,0.));
#6900=DIRECTION('ref_axis',(1.,0.,0.));
#6901=DIRECTION('',(-0.707106781186547,0.707106781186548,-8.65956056235493E-17));
#6902=DIRECTION('center_axis',(0.,-1.,0.));
#6903=DIRECTION('ref_axis',(0.,0.,-1.));
#6904=DIRECTION('center_axis',(0.866025403784439,0.,-0.5));
#6905=DIRECTION('ref_axis',(0.5,0.,0.866025403784439));
#6906=DIRECTION('',(-0.5,0.,-0.866025403784439));
#6907=DIRECTION('',(0.,-1.,0.));
#6908=DIRECTION('',(0.5,0.,0.866025403784439));
#6909=DIRECTION('',(0.,-1.,0.));
#6910=DIRECTION('center_axis',(1.60246890531964E-16,0.,-1.));
#6911=DIRECTION('ref_axis',(1.,0.,1.60246890531964E-16));
#6912=DIRECTION('',(-1.,0.,-1.60246890531964E-16));
#6913=DIRECTION('',(0.,-1.,0.));
#6914=DIRECTION('',(1.,0.,1.60246890531964E-16));
#6915=DIRECTION('center_axis',(-0.866025403784439,0.,-0.5));
#6916=DIRECTION('ref_axis',(0.5,0.,-0.866025403784439));
#6917=DIRECTION('',(-0.5,0.,0.866025403784439));
#6918=DIRECTION('',(0.,-1.,0.));
#6919=DIRECTION('',(0.5,0.,-0.866025403784439));
#6920=DIRECTION('center_axis',(-0.866025403784439,0.,0.5));
#6921=DIRECTION('ref_axis',(-0.5,0.,-0.866025403784439));
#6922=DIRECTION('',(0.5,0.,0.866025403784439));
#6923=DIRECTION('',(0.,-1.,0.));
#6924=DIRECTION('',(-0.5,0.,-0.866025403784439));
#6925=DIRECTION('center_axis',(-1.60246890531964E-16,0.,1.));
#6926=DIRECTION('ref_axis',(-1.,0.,-1.60246890531964E-16));
#6927=DIRECTION('',(1.,0.,1.60246890531964E-16));
#6928=DIRECTION('',(0.,-1.,0.));
#6929=DIRECTION('',(-1.,0.,-1.60246890531964E-16));
#6930=DIRECTION('center_axis',(0.866025403784439,0.,0.5));
#6931=DIRECTION('ref_axis',(-0.5,0.,0.866025403784439));
#6932=DIRECTION('',(0.5,0.,-0.866025403784439));
#6933=DIRECTION('',(-0.5,0.,0.866025403784439));
#6934=DIRECTION('center_axis',(0.,1.,0.));
#6935=DIRECTION('ref_axis',(1.,0.,0.));
#6936=DIRECTION('center_axis',(0.,-1.,0.));
#6937=DIRECTION('ref_axis',(0.,0.,-1.));
#6938=DIRECTION('',(0.,0.,1.));
#6939=DIRECTION('',(1.,0.,0.));
#6940=DIRECTION('',(0.,0.,1.));
#6941=DIRECTION('',(1.,0.,0.));
#6942=DIRECTION('',(0.,0.,1.));
#6943=DIRECTION('',(1.,0.,0.));
#6944=DIRECTION('',(0.,0.,1.));
#6945=DIRECTION('',(1.,0.,0.));
#6946=DIRECTION('',(0.,0.,1.));
#6947=DIRECTION('',(1.,0.,0.));
#6948=DIRECTION('',(0.,0.,1.));
#6949=DIRECTION('',(2.22044604925031E-16,-1.,0.));
#6950=DIRECTION('',(0.,0.,1.));
#6951=DIRECTION('',(2.22044604925031E-16,-1.,0.));
#6952=DIRECTION('',(0.,0.,1.));
#6953=DIRECTION('',(1.,0.,0.));
#6954=DIRECTION('',(0.,0.,1.));
#6955=DIRECTION('',(1.,0.,0.));
#6956=DIRECTION('',(0.,0.,1.));
#6957=DIRECTION('',(1.,0.,0.));
#6958=DIRECTION('',(0.,0.,1.));
#6959=DIRECTION('',(1.,0.,0.));
#6960=DIRECTION('',(0.,0.,1.));
#6961=DIRECTION('',(1.,0.,0.));
#6962=DIRECTION('',(0.,0.,1.));
#6963=DIRECTION('',(1.,0.,0.));
#6964=DIRECTION('',(0.,0.,1.));
#6965=DIRECTION('',(1.,0.,0.));
#6966=DIRECTION('',(0.,0.,1.));
#6967=DIRECTION('',(1.,0.,0.));
#6968=DIRECTION('',(0.,0.,1.));
#6969=DIRECTION('',(1.,0.,0.));
#6970=DIRECTION('',(0.,0.,1.));
#6971=DIRECTION('',(1.,0.,0.));
#6972=DIRECTION('',(0.,-1.,2.22044604925031E-16));
#6973=DIRECTION('',(1.,0.,0.));
#6974=DIRECTION('',(0.,-1.,2.22044604925031E-16));
#6975=DIRECTION('',(1.,0.,0.));
#6976=DIRECTION('',(0.,-1.,2.22044604925031E-16));
#6977=DIRECTION('',(1.,0.,0.));
#6978=DIRECTION('',(0.,-1.,2.22044604925031E-16));
#6979=DIRECTION('',(1.,0.,0.));
#6980=DIRECTION('',(0.,-1.,2.22044604925031E-16));
#6981=DIRECTION('',(1.,0.,0.));
#6982=DIRECTION('',(0.,-1.,2.22044604925031E-16));
#6983=DIRECTION('',(1.,0.,0.));
#6984=DIRECTION('',(0.,-1.,2.22044604925031E-16));
#6985=DIRECTION('',(1.,0.,0.));
#6986=DIRECTION('',(0.,-1.,2.22044604925031E-16));
#6987=DIRECTION('',(1.,0.,0.));
#6988=DIRECTION('',(0.,0.,1.));
#6989=DIRECTION('',(1.,0.,0.));
#6990=DIRECTION('',(0.,1.,2.22044604925031E-16));
#6991=DIRECTION('',(1.,0.,0.));
#6992=DIRECTION('',(0.,1.,2.22044604925031E-16));
#6993=DIRECTION('',(1.,0.,0.));
#6994=DIRECTION('',(0.,1.,2.22044604925031E-16));
#6995=DIRECTION('',(1.,0.,0.));
#6996=DIRECTION('',(0.,1.,2.22044604925031E-16));
#6997=DIRECTION('',(1.,0.,0.));
#6998=DIRECTION('',(0.,-1.,2.22044604925031E-16));
#6999=DIRECTION('',(1.,0.,0.));
#7000=DIRECTION('',(0.,0.,1.));
#7001=DIRECTION('',(1.,0.,0.));
#7002=DIRECTION('',(0.,1.,2.22044604925031E-16));
#7003=DIRECTION('',(1.,0.,0.));
#7004=DIRECTION('',(0.,0.,1.));
#7005=DIRECTION('',(1.,0.,0.));
#7006=DIRECTION('',(0.,1.,2.22044604925031E-16));
#7007=DIRECTION('',(1.,0.,0.));
#7008=CARTESIAN_POINT('',(0.,0.,0.));
#7009=CARTESIAN_POINT('',(0.,0.,0.));
#7010=CARTESIAN_POINT('Origin',(-4.,0.,0.9));
#7011=CARTESIAN_POINT('',(-4.165,-2.02066721859313E-17,1.));
#7012=CARTESIAN_POINT('Origin',(-4.,0.,1.));
#7013=CARTESIAN_POINT('',(-4.165,-3.78589117085946E-17,1.615));
#7014=CARTESIAN_POINT('',(-4.165,-2.02066721859313E-17,0.9));
#7015=CARTESIAN_POINT('',(-4.,-0.165,1.63516919445621));
#7016=CARTESIAN_POINT('Ctrl Pts',(-4.,-0.165,1.63516919445621));
#7017=CARTESIAN_POINT('Ctrl Pts',(-4.02080740660683,-0.165,1.63516919445621));
#7018=CARTESIAN_POINT('Ctrl Pts',(-4.0429430103202,-0.160824823566189,1.63409071616177));
#7019=CARTESIAN_POINT('Ctrl Pts',(-4.08356969606673,-0.14396122454405,1.63024260952261));
#7020=CARTESIAN_POINT('Ctrl Pts',(-4.10206824127575,-0.131276996515812,
1.62753363614987));
#7021=CARTESIAN_POINT('Ctrl Pts',(-4.13127524440319,-0.102069993388373,
1.62248518534955));
#7022=CARTESIAN_POINT('Ctrl Pts',(-4.14396083991376,-0.0835707156017109,
1.61981093112785));
#7023=CARTESIAN_POINT('Ctrl Pts',(-4.16082543577155,-0.0429414425249984,
1.61604293526104));
#7024=CARTESIAN_POINT('Ctrl Pts',(-4.165,-0.0208049103060176,1.615));
#7025=CARTESIAN_POINT('Ctrl Pts',(-4.165,1.38777878078145E-17,1.615));
#7026=CARTESIAN_POINT('Ctrl Pts',(-4.165,-1.73472347597681E-17,1.615));
#7027=CARTESIAN_POINT('Ctrl Pts',(-4.165,0.0208049103060176,1.615));
#7028=CARTESIAN_POINT('Ctrl Pts',(-4.16082543577155,0.0429414425249979,
1.61604293526104));
#7029=CARTESIAN_POINT('Ctrl Pts',(-4.14396083991376,0.0835707156017106,
1.61981093112785));
#7030=CARTESIAN_POINT('Ctrl Pts',(-4.13127524440319,0.102069993388373,1.62248518534955));
#7031=CARTESIAN_POINT('Ctrl Pts',(-4.10206824127575,0.131276996515812,1.62753363614987));
#7032=CARTESIAN_POINT('Ctrl Pts',(-4.08356969606673,0.14396122454405,1.63024260952261));
#7033=CARTESIAN_POINT('Ctrl Pts',(-4.0429430103202,0.160824823566189,1.63409071616177));
#7034=CARTESIAN_POINT('Ctrl Pts',(-4.02080740660683,0.165,1.63516919445621));
#7035=CARTESIAN_POINT('Ctrl Pts',(-3.97919259339316,0.165,1.63516919445621));
#7036=CARTESIAN_POINT('Ctrl Pts',(-3.9570569896798,0.160824823566189,1.63409071616177));
#7037=CARTESIAN_POINT('Ctrl Pts',(-3.91643030393327,0.143961224544049,1.63024260952261));
#7038=CARTESIAN_POINT('Ctrl Pts',(-3.89793175872425,0.131276996515812,1.62753363614987));
#7039=CARTESIAN_POINT('Ctrl Pts',(-3.86872475559681,0.102069993388373,1.62248518534955));
#7040=CARTESIAN_POINT('Ctrl Pts',(-3.85603916008624,0.0835707156017107,
1.61981093112785));
#7041=CARTESIAN_POINT('Ctrl Pts',(-3.83917456422845,0.0429414425249981,
1.61604293526104));
#7042=CARTESIAN_POINT('Ctrl Pts',(-3.835,0.0208049103060177,1.615));
#7043=CARTESIAN_POINT('Ctrl Pts',(-3.835,-0.0208049103060176,1.615));
#7044=CARTESIAN_POINT('Ctrl Pts',(-3.83917456422845,-0.042941442524998,
1.61604293526104));
#7045=CARTESIAN_POINT('Ctrl Pts',(-3.85603916008624,-0.0835707156017107,
1.61981093112785));
#7046=CARTESIAN_POINT('Ctrl Pts',(-3.86872475559681,-0.102069993388373,
1.62248518534955));
#7047=CARTESIAN_POINT('Ctrl Pts',(-3.89793175872425,-0.131276996515812,
1.62753363614987));
#7048=CARTESIAN_POINT('Ctrl Pts',(-3.91643030393327,-0.143961224544049,
1.63024260952261));
#7049=CARTESIAN_POINT('Ctrl Pts',(-3.9570569896798,-0.160824823566189,1.63409071616177));
#7050=CARTESIAN_POINT('Ctrl Pts',(-3.97919259339316,-0.165,1.63516919445621));
#7051=CARTESIAN_POINT('Ctrl Pts',(-4.,-0.165,1.63516919445621));
#7052=CARTESIAN_POINT('Origin',(4.,0.,0.9));
#7053=CARTESIAN_POINT('',(3.835,-2.02066721859313E-17,1.));
#7054=CARTESIAN_POINT('Origin',(4.,0.,1.));
#7055=CARTESIAN_POINT('',(3.835,-2.02066721859313E-17,2.1));
#7056=CARTESIAN_POINT('',(3.835,-2.02066721859313E-17,0.9));
#7057=CARTESIAN_POINT('Origin',(4.,0.,2.1));
#7058=CARTESIAN_POINT('Origin',(4.,0.,2.1));
#7059=CARTESIAN_POINT('Origin',(-2.05060966544099,-2.05060966544099,1.3));
#7060=CARTESIAN_POINT('',(-2.21560966544099,-2.05060966544099,1.4));
#7061=CARTESIAN_POINT('Origin',(-2.05060966544099,-2.05060966544099,1.4));
#7062=CARTESIAN_POINT('',(-2.21560966544099,-2.05060966544099,2.7));
#7063=CARTESIAN_POINT('',(-2.21560966544099,-2.05060966544099,1.3));
#7064=CARTESIAN_POINT('Origin',(-2.05060966544099,-2.05060966544099,2.7));
#7065=CARTESIAN_POINT('Origin',(-2.05060966544099,-2.05060966544099,2.7));
#7066=CARTESIAN_POINT('Origin',(-2.05060966544099,2.05060966544099,1.3));
#7067=CARTESIAN_POINT('',(-2.21560966544099,2.05060966544099,1.4));
#7068=CARTESIAN_POINT('Origin',(-2.05060966544099,2.05060966544099,1.4));
#7069=CARTESIAN_POINT('',(-2.21560966544099,2.05060966544099,2.7));
#7070=CARTESIAN_POINT('',(-2.21560966544099,2.05060966544099,1.3));
#7071=CARTESIAN_POINT('Origin',(-2.05060966544099,2.05060966544099,2.7));
#7072=CARTESIAN_POINT('Origin',(-2.05060966544099,2.05060966544099,2.7));
#7073=CARTESIAN_POINT('Origin',(2.05060966544099,2.05060966544099,1.3));
#7074=CARTESIAN_POINT('',(1.88560966544099,2.05060966544099,1.4));
#7075=CARTESIAN_POINT('Origin',(2.05060966544099,2.05060966544099,1.4));
#7076=CARTESIAN_POINT('',(1.88560966544099,2.05060966544099,2.7));
#7077=CARTESIAN_POINT('',(1.88560966544099,2.05060966544099,1.3));
#7078=CARTESIAN_POINT('Origin',(2.05060966544099,2.05060966544099,2.7));
#7079=CARTESIAN_POINT('Origin',(2.05060966544099,2.05060966544099,2.7));
#7080=CARTESIAN_POINT('Origin',(2.05060966544099,-2.05060966544099,1.3));
#7081=CARTESIAN_POINT('',(1.88560966544099,-2.05060966544099,1.4));
#7082=CARTESIAN_POINT('Origin',(2.05060966544099,-2.05060966544099,1.4));
#7083=CARTESIAN_POINT('',(1.88560966544099,-2.05060966544099,2.7));
#7084=CARTESIAN_POINT('',(1.88560966544099,-2.05060966544099,1.3));
#7085=CARTESIAN_POINT('Origin',(2.05060966544099,-2.05060966544099,2.7));
#7086=CARTESIAN_POINT('Origin',(2.05060966544099,-2.05060966544099,2.7));
#7087=CARTESIAN_POINT('Origin',(0.,0.,1.4));
#7088=CARTESIAN_POINT('',(-2.24,-2.74320883009007E-16,1.4));
#7089=CARTESIAN_POINT('Origin',(0.,0.,1.4));
#7090=CARTESIAN_POINT('',(-2.24,-2.74320883009007E-16,1.51));
#7091=CARTESIAN_POINT('',(-2.24,-2.74320883009007E-16,1.4));
#7092=CARTESIAN_POINT('Origin',(0.,0.,1.51));
#7093=CARTESIAN_POINT('Origin',(0.,0.,1.4));
#7094=CARTESIAN_POINT('',(-2.46,-3.01263112590249E-16,1.4));
#7095=CARTESIAN_POINT('Origin',(0.,0.,1.4));
#7096=CARTESIAN_POINT('',(-2.46,-3.01263112590249E-16,1.51));
#7097=CARTESIAN_POINT('',(-2.46,-3.01263112590249E-16,1.4));
#7098=CARTESIAN_POINT('Origin',(0.,0.,1.51));
#7099=CARTESIAN_POINT('Origin',(0.,0.,1.51));
#7100=CARTESIAN_POINT('Origin',(0.,0.,1.4));
#7101=CARTESIAN_POINT('',(-3.31,-4.05358090517774E-16,1.4));
#7102=CARTESIAN_POINT('Origin',(0.,0.,1.4));
#7103=CARTESIAN_POINT('Origin',(-6.38378239159465E-16,-3.4,3.5));
#7104=CARTESIAN_POINT('',(0.184661853126193,-3.5,3.5));
#7105=CARTESIAN_POINT('',(-0.184661853126194,-3.5,3.5));
#7106=CARTESIAN_POINT('',(-3.19189119579733E-16,-3.5,3.5));
#7107=CARTESIAN_POINT('',(-0.210000000000001,-3.4,3.5));
#7108=CARTESIAN_POINT('Origin',(-6.2456986756515E-16,-3.4,3.5));
#7109=CARTESIAN_POINT('Origin',(-6.2456986756515E-16,-3.4,3.5));
#7110=CARTESIAN_POINT('Origin',(-6.2456986756515E-16,-3.4,3.5));
#7111=CARTESIAN_POINT('',(0.184661853126193,-3.5,3.55964005336244));
#7112=CARTESIAN_POINT('',(0.184661853126193,-3.5,3.5));
#7113=CARTESIAN_POINT('',(-0.184661853126194,-3.5,3.55964005336244));
#7114=CARTESIAN_POINT('Ctrl Pts',(-0.184661853126194,-3.5,3.55964005336244));
#7115=CARTESIAN_POINT('Ctrl Pts',(-0.174800846718384,-3.51820951716955,
3.56240057663217));
#7116=CARTESIAN_POINT('Ctrl Pts',(-0.162284556957793,-3.53470029114056,
3.56564880027768));
#7117=CARTESIAN_POINT('Ctrl Pts',(-0.129946422600616,-3.56703842549773,
3.57282972708545));
#7118=CARTESIAN_POINT('Ctrl Pts',(-0.106445900548852,-3.58317393160533,
3.57717919558841));
#7119=CARTESIAN_POINT('Ctrl Pts',(-0.054753956552258,-3.60465928779521,
3.58330402961894));
#7120=CARTESIAN_POINT('Ctrl Pts',(-0.0265493609398035,-3.61,3.585));
#7121=CARTESIAN_POINT('Ctrl Pts',(0.0265493609398022,-3.61,3.585));
#7122=CARTESIAN_POINT('Ctrl Pts',(0.0547539565522566,-3.60465928779521,
3.58330402961894));
#7123=CARTESIAN_POINT('Ctrl Pts',(0.106445900548851,-3.58317393160533,3.57717919558841));
#7124=CARTESIAN_POINT('Ctrl Pts',(0.129946422600615,-3.56703842549773,3.57282972708545));
#7125=CARTESIAN_POINT('Ctrl Pts',(0.162284556957791,-3.53470029114056,3.56564880027768));
#7126=CARTESIAN_POINT('Ctrl Pts',(0.174800846718383,-3.51820951716955,3.56240057663217));
#7127=CARTESIAN_POINT('Ctrl Pts',(0.184661853126193,-3.5,3.55964005336244));
#7128=CARTESIAN_POINT('',(-0.184661853126194,-3.5,3.5));
#7129=CARTESIAN_POINT('',(-0.210000000000001,-3.4,5.));
#7130=CARTESIAN_POINT('',(-0.210000000000001,-3.4,3.5));
#7131=CARTESIAN_POINT('Origin',(-6.2456986756515E-16,-3.4,5.));
#7132=CARTESIAN_POINT('Origin',(2.94448637286709,1.7,3.5));
#7133=CARTESIAN_POINT('',(2.73448637286709,1.7,3.5));
#7134=CARTESIAN_POINT('Origin',(2.94448637286709,1.7,3.5));
#7135=CARTESIAN_POINT('',(2.73448637286709,1.7,5.));
#7136=CARTESIAN_POINT('',(2.73448637286709,1.7,3.5));
#7137=CARTESIAN_POINT('Origin',(2.94448637286709,1.7,5.));
#7138=CARTESIAN_POINT('Origin',(2.94448637286709,1.7,3.5));
#7139=CARTESIAN_POINT('Origin',(2.0818995585505E-16,3.4,3.5));
#7140=CARTESIAN_POINT('',(-0.21,3.4,3.5));
#7141=CARTESIAN_POINT('Origin',(2.0818995585505E-16,3.4,3.5));
#7142=CARTESIAN_POINT('',(-0.21,3.4,5.));
#7143=CARTESIAN_POINT('',(-0.21,3.4,3.5));
#7144=CARTESIAN_POINT('Origin',(2.0818995585505E-16,3.4,5.));
#7145=CARTESIAN_POINT('Origin',(2.22044604925031E-16,3.4,3.5));
#7146=CARTESIAN_POINT('Origin',(-2.94448637286709,1.7,3.5));
#7147=CARTESIAN_POINT('',(-3.15448637286709,1.7,3.5));
#7148=CARTESIAN_POINT('Origin',(-2.94448637286709,1.7,3.5));
#7149=CARTESIAN_POINT('',(-3.15448637286709,1.7,5.));
#7150=CARTESIAN_POINT('',(-3.15448637286709,1.7,3.5));
#7151=CARTESIAN_POINT('Origin',(-2.94448637286709,1.7,5.));
#7152=CARTESIAN_POINT('Origin',(-2.94448637286709,1.7,3.5));
#7153=CARTESIAN_POINT('Origin',(-2.94448637286709,-1.7,3.5));
#7154=CARTESIAN_POINT('',(-3.15448637286709,-1.7,3.5));
#7155=CARTESIAN_POINT('Origin',(-2.94448637286709,-1.7,3.5));
#7156=CARTESIAN_POINT('',(-3.15448637286709,-1.7,5.));
#7157=CARTESIAN_POINT('',(-3.15448637286709,-1.7,3.5));
#7158=CARTESIAN_POINT('Origin',(-2.94448637286709,-1.7,5.));
#7159=CARTESIAN_POINT('Origin',(-2.94448637286709,-1.7,3.5));
#7160=CARTESIAN_POINT('Origin',(2.94448637286709,-1.7,3.5));
#7161=CARTESIAN_POINT('',(2.73448637286709,-1.7,3.5));
#7162=CARTESIAN_POINT('Origin',(2.94448637286709,-1.7,3.5));
#7163=CARTESIAN_POINT('',(2.73448637286709,-1.7,5.));
#7164=CARTESIAN_POINT('',(2.73448637286709,-1.7,3.5));
#7165=CARTESIAN_POINT('Origin',(2.94448637286709,-1.7,5.));
#7166=CARTESIAN_POINT('Origin',(2.94448637286709,-1.7,3.5));
#7167=CARTESIAN_POINT('Origin',(0.,-3.5,2.9));
#7168=CARTESIAN_POINT('',(-0.685,-3.5,2.9));
#7169=CARTESIAN_POINT('Origin',(0.,-3.5,2.9));
#7170=CARTESIAN_POINT('Origin',(0.,-3.5,2.9));
#7171=CARTESIAN_POINT('',(-0.2,-3.5,2.9));
#7172=CARTESIAN_POINT('Origin',(0.,-3.5,2.9));
#7173=CARTESIAN_POINT('Origin',(0.,-2.,2.8));
#7174=CARTESIAN_POINT('',(-0.173205080756888,-1.9,2.8));
#7175=CARTESIAN_POINT('',(-0.173205080756888,-2.1,2.8));
#7176=CARTESIAN_POINT('',(-0.173205080756888,-3.6,2.8));
#7177=CARTESIAN_POINT('Origin',(0.,-2.,2.8));
#7178=CARTESIAN_POINT('Origin',(0.,-2.,2.8));
#7179=CARTESIAN_POINT('',(0.173205080756888,-2.1,2.8));
#7180=CARTESIAN_POINT('',(0.173205080756888,-1.9,2.8));
#7181=CARTESIAN_POINT('',(0.173205080756888,-3.6,2.8));
#7182=CARTESIAN_POINT('Origin',(0.,-2.,2.8));
#7183=CARTESIAN_POINT('Origin',(0.,-2.,2.8));
#7184=CARTESIAN_POINT('',(-0.2,-2.,2.9));
#7185=CARTESIAN_POINT('Origin',(0.,-2.,2.9));
#7186=CARTESIAN_POINT('Origin',(0.,-2.,2.9));
#7187=CARTESIAN_POINT('Origin',(0.,-2.,2.8));
#7188=CARTESIAN_POINT('',(0.2,-2.,2.9));
#7189=CARTESIAN_POINT('Origin',(0.,-2.,2.9));
#7190=CARTESIAN_POINT('Origin',(0.,-2.,2.9));
#7191=CARTESIAN_POINT('Origin',(0.,-2.,2.8));
#7192=CARTESIAN_POINT('Origin',(0.,-2.,2.9));
#7193=CARTESIAN_POINT('',(-0.2,-2.,3.2));
#7194=CARTESIAN_POINT('',(-0.2,-2.,2.8));
#7195=CARTESIAN_POINT('Origin',(0.,-2.,3.2));
#7196=CARTESIAN_POINT('Origin',(0.,-2.,2.9));
#7197=CARTESIAN_POINT('Origin',(0.,-3.6,2.9));
#7198=CARTESIAN_POINT('',(-0.2,-3.6,2.9));
#7199=CARTESIAN_POINT('',(-0.2,-0.565685424949238,2.9));
#7200=CARTESIAN_POINT('',(-0.2,-3.6,2.9));
#7201=CARTESIAN_POINT('Ctrl Pts',(-0.2,-0.565685424949238,2.9));
#7202=CARTESIAN_POINT('Ctrl Pts',(-0.2,-0.565685424949238,2.87467078791842));
#7203=CARTESIAN_POINT('Ctrl Pts',(-0.194898067853762,-0.567565356574251,
2.8477996053073));
#7204=CARTESIAN_POINT('Ctrl Pts',(-0.17443058152527,-0.574186082552466,
2.79858936400846));
#7205=CARTESIAN_POINT('Ctrl Pts',(-0.159074095999941,-0.578813771212596,
2.77623138352532));
#7206=CARTESIAN_POINT('Ctrl Pts',(-0.123776803829002,-0.587374622031365,
2.74093409135438));
#7207=CARTESIAN_POINT('Ctrl Pts',(-0.101415562391481,-0.59188739106068,
2.72557130277668));
#7208=CARTESIAN_POINT('Ctrl Pts',(-0.0521932274441715,-0.598240475886912,
2.70509911583939));
#7209=CARTESIAN_POINT('Ctrl Pts',(-0.0253174643734703,-0.6,2.7));
#7210=CARTESIAN_POINT('Ctrl Pts',(0.0253174643734703,-0.6,2.7));
#7211=CARTESIAN_POINT('Ctrl Pts',(0.0521932274441715,-0.598240475886912,
2.70509911583939));
#7212=CARTESIAN_POINT('Ctrl Pts',(0.101415562391481,-0.59188739106068,2.72557130277668));
#7213=CARTESIAN_POINT('Ctrl Pts',(0.123776803829002,-0.587374622031365,
2.74093409135438));
#7214=CARTESIAN_POINT('Ctrl Pts',(0.159074095999941,-0.578813771212596,
2.77623138352532));
#7215=CARTESIAN_POINT('Ctrl Pts',(0.17443058152527,-0.574186082552466,2.79858936400846));
#7216=CARTESIAN_POINT('Ctrl Pts',(0.194898067853762,-0.567565356574251,
2.8477996053073));
#7217=CARTESIAN_POINT('Ctrl Pts',(0.2,-0.565685424949238,2.87467078791842));
#7218=CARTESIAN_POINT('Ctrl Pts',(0.2,-0.565685424949238,2.92532921208158));
#7219=CARTESIAN_POINT('Ctrl Pts',(0.194898067853762,-0.567565356574251,
2.9522003946927));
#7220=CARTESIAN_POINT('Ctrl Pts',(0.17443058152527,-0.574186082552466,3.00141063599154));
#7221=CARTESIAN_POINT('Ctrl Pts',(0.159074095999941,-0.578813771212596,
3.02376861647468));
#7222=CARTESIAN_POINT('Ctrl Pts',(0.123776803829002,-0.587374622031365,
3.05906590864562));
#7223=CARTESIAN_POINT('Ctrl Pts',(0.101415562391481,-0.59188739106068,3.07442869722332));
#7224=CARTESIAN_POINT('Ctrl Pts',(0.052193227444171,-0.598240475886912,
3.09490088416061));
#7225=CARTESIAN_POINT('Ctrl Pts',(0.0253174643734703,-0.6,3.1));
#7226=CARTESIAN_POINT('Ctrl Pts',(-0.0253174643734703,-0.6,3.1));
#7227=CARTESIAN_POINT('Ctrl Pts',(-0.052193227444171,-0.598240475886912,
3.09490088416061));
#7228=CARTESIAN_POINT('Ctrl Pts',(-0.101415562391481,-0.59188739106068,
3.07442869722332));
#7229=CARTESIAN_POINT('Ctrl Pts',(-0.123776803829002,-0.587374622031365,
3.05906590864562));
#7230=CARTESIAN_POINT('Ctrl Pts',(-0.159074095999941,-0.578813771212596,
3.02376861647468));
#7231=CARTESIAN_POINT('Ctrl Pts',(-0.17443058152527,-0.574186082552466,
3.00141063599154));
#7232=CARTESIAN_POINT('Ctrl Pts',(-0.194898067853762,-0.567565356574251,
2.9522003946927));
#7233=CARTESIAN_POINT('Ctrl Pts',(-0.2,-0.565685424949238,2.92532921208158));
#7234=CARTESIAN_POINT('Ctrl Pts',(-0.2,-0.565685424949238,2.9));
#7235=CARTESIAN_POINT('Origin',(0.,-4.6,2.9));
#7236=CARTESIAN_POINT('',(-0.685,-4.44755831889813,2.9));
#7237=CARTESIAN_POINT('Ctrl Pts',(-0.685,-4.44755831889813,2.9));
#7238=CARTESIAN_POINT('Ctrl Pts',(-0.685,-4.44755831889813,2.98615495576053));
#7239=CARTESIAN_POINT('Ctrl Pts',(-0.667754444280465,-4.4503204226392,3.07795945171461));
#7240=CARTESIAN_POINT('Ctrl Pts',(-0.597806423657171,-4.46025507446226,
3.24668870614449));
#7241=CARTESIAN_POINT('Ctrl Pts',(-0.545111157186078,-4.46727957365527,
3.32362513303949));
#7242=CARTESIAN_POINT('Ctrl Pts',(-0.42362625704472,-4.48043230270009,3.44511003318085));
#7243=CARTESIAN_POINT('Ctrl Pts',(-0.346689345476453,-4.48742111878839,
3.49780618135505));
#7244=CARTESIAN_POINT('Ctrl Pts',(-0.177958434129502,-4.49727390705164,
3.56775484339031));
#7245=CARTESIAN_POINT('Ctrl Pts',(-0.0861533615257771,-4.5,3.585));
#7246=CARTESIAN_POINT('Ctrl Pts',(0.0861533615257768,-4.5,3.585));
#7247=CARTESIAN_POINT('Ctrl Pts',(0.177958434129502,-4.49727390705164,3.56775484339031));
#7248=CARTESIAN_POINT('Ctrl Pts',(0.346689345476453,-4.48742111878839,3.49780618135505));
#7249=CARTESIAN_POINT('Ctrl Pts',(0.42362625704472,-4.48043230270009,3.44511003318085));
#7250=CARTESIAN_POINT('Ctrl Pts',(0.545111157186078,-4.46727957365527,3.32362513303949));
#7251=CARTESIAN_POINT('Ctrl Pts',(0.59780642365717,-4.46025507446226,3.24668870614449));
#7252=CARTESIAN_POINT('Ctrl Pts',(0.667754444280465,-4.4503204226392,3.07795945171461));
#7253=CARTESIAN_POINT('Ctrl Pts',(0.685,-4.44755831889813,2.98615495576053));
#7254=CARTESIAN_POINT('Ctrl Pts',(0.685,-4.44755831889813,2.81384504423947));
#7255=CARTESIAN_POINT('Ctrl Pts',(0.667754444280465,-4.4503204226392,2.72204054828539));
#7256=CARTESIAN_POINT('Ctrl Pts',(0.597806423657171,-4.46025507446226,2.55331129385551));
#7257=CARTESIAN_POINT('Ctrl Pts',(0.545111157186078,-4.46727957365527,2.47637486696051));
#7258=CARTESIAN_POINT('Ctrl Pts',(0.42362625704472,-4.48043230270009,2.35488996681915));
#7259=CARTESIAN_POINT('Ctrl Pts',(0.346689345476454,-4.48742111878839,2.30219381864495));
#7260=CARTESIAN_POINT('Ctrl Pts',(0.177958434129502,-4.49727390705164,2.23224515660969));
#7261=CARTESIAN_POINT('Ctrl Pts',(0.0861533615257774,-4.5,2.215));
#7262=CARTESIAN_POINT('Ctrl Pts',(-0.0861533615257767,-4.5,2.215));
#7263=CARTESIAN_POINT('Ctrl Pts',(-0.177958434129502,-4.49727390705164,
2.23224515660969));
#7264=CARTESIAN_POINT('Ctrl Pts',(-0.346689345476453,-4.48742111878839,
2.30219381864495));
#7265=CARTESIAN_POINT('Ctrl Pts',(-0.423626257044719,-4.48043230270009,
2.35488996681915));
#7266=CARTESIAN_POINT('Ctrl Pts',(-0.545111157186078,-4.46727957365527,
2.47637486696051));
#7267=CARTESIAN_POINT('Ctrl Pts',(-0.59780642365717,-4.46025507446226,2.55331129385551));
#7268=CARTESIAN_POINT('Ctrl Pts',(-0.667754444280465,-4.4503204226392,2.72204054828539));
#7269=CARTESIAN_POINT('Ctrl Pts',(-0.685,-4.44755831889813,2.81384504423947));
#7270=CARTESIAN_POINT('Ctrl Pts',(-0.685,-4.44755831889813,2.9));
#7271=CARTESIAN_POINT('',(-0.685,-4.6,2.9));
#7272=CARTESIAN_POINT('Origin',(-0.1,0.,3.9));
#7273=CARTESIAN_POINT('',(2.46779253585061,0.4,3.9));
#7274=CARTESIAN_POINT('',(2.5,-3.67625427122537E-18,4.3));
#7275=CARTESIAN_POINT('Ctrl Pts',(2.46779253585061,0.4,3.9));
#7276=CARTESIAN_POINT('Ctrl Pts',(2.46779253585061,0.4,3.95031849222446));
#7277=CARTESIAN_POINT('Ctrl Pts',(2.46949065540042,0.389926098864548,4.00393070664371));
#7278=CARTESIAN_POINT('Ctrl Pts',(2.47559507764305,0.3490780234852,4.10245615200085));
#7279=CARTESIAN_POINT('Ctrl Pts',(2.47991004659989,0.318308483288254,4.14737694166098));
#7280=CARTESIAN_POINT('Ctrl Pts',(2.48798680132732,0.247377744540872,4.21830768040837));
#7281=CARTESIAN_POINT('Ctrl Pts',(2.49227754123301,0.202456609487086,4.24907785041389));
#7282=CARTESIAN_POINT('Ctrl Pts',(2.49832635585429,0.103929980260481,4.28992638341895));
#7283=CARTESIAN_POINT('Ctrl Pts',(2.5,0.0503173531062475,4.3));
#7284=CARTESIAN_POINT('Ctrl Pts',(2.5,8.32667268468867E-17,4.3));
#7285=CARTESIAN_POINT('Ctrl Pts',(2.5,2.77555756156289E-17,4.3));
#7286=CARTESIAN_POINT('Ctrl Pts',(2.5,-0.0503173531062473,4.3));
#7287=CARTESIAN_POINT('Ctrl Pts',(2.49832635585429,-0.103929980260481,4.28992638341895));
#7288=CARTESIAN_POINT('Ctrl Pts',(2.49227754123301,-0.202456609487086,4.24907785041389));
#7289=CARTESIAN_POINT('Ctrl Pts',(2.48798680132732,-0.247377744540872,4.21830768040837));
#7290=CARTESIAN_POINT('Ctrl Pts',(2.47991004659989,-0.318308483288254,4.14737694166098));
#7291=CARTESIAN_POINT('Ctrl Pts',(2.47559507764305,-0.3490780234852,4.10245615200085));
#7292=CARTESIAN_POINT('Ctrl Pts',(2.46949065540042,-0.389926098864548,4.00393070664371));
#7293=CARTESIAN_POINT('Ctrl Pts',(2.46779253585061,-0.4,3.95031849222446));
#7294=CARTESIAN_POINT('Ctrl Pts',(2.46779253585061,-0.4,3.84968150777554));
#7295=CARTESIAN_POINT('Ctrl Pts',(2.46949065540042,-0.389926098864548,3.79606929335629));
#7296=CARTESIAN_POINT('Ctrl Pts',(2.47559507764305,-0.3490780234852,3.69754384799915));
#7297=CARTESIAN_POINT('Ctrl Pts',(2.47991004659989,-0.318308483288254,3.65262305833902));
#7298=CARTESIAN_POINT('Ctrl Pts',(2.48798680132732,-0.247377744540872,3.58169231959163));
#7299=CARTESIAN_POINT('Ctrl Pts',(2.49227754123301,-0.202456609487086,3.55092214958611));
#7300=CARTESIAN_POINT('Ctrl Pts',(2.49832635585429,-0.103929980260481,3.51007361658105));
#7301=CARTESIAN_POINT('Ctrl Pts',(2.5,-0.0503173531062475,3.5));
#7302=CARTESIAN_POINT('Ctrl Pts',(2.5,0.0503173531062473,3.5));
#7303=CARTESIAN_POINT('Ctrl Pts',(2.49832635585429,0.103929980260481,3.51007361658105));
#7304=CARTESIAN_POINT('Ctrl Pts',(2.49227754123301,0.202456609487086,3.55092214958611));
#7305=CARTESIAN_POINT('Ctrl Pts',(2.48798680132732,0.247377744540872,3.58169231959163));
#7306=CARTESIAN_POINT('Ctrl Pts',(2.47991004659989,0.318308483288254,3.65262305833902));
#7307=CARTESIAN_POINT('Ctrl Pts',(2.47559507764305,0.3490780234852,3.69754384799915));
#7308=CARTESIAN_POINT('Ctrl Pts',(2.46949065540042,0.389926098864548,3.79606929335629));
#7309=CARTESIAN_POINT('Ctrl Pts',(2.46779253585061,0.4,3.84968150777554));
#7310=CARTESIAN_POINT('Ctrl Pts',(2.46779253585061,0.4,3.9));
#7311=CARTESIAN_POINT('',(3.,4.89858719658941E-17,4.3));
#7312=CARTESIAN_POINT('',(-0.1,-4.89858719658941E-17,4.3));
#7313=CARTESIAN_POINT('Origin',(3.,0.,3.9));
#7314=CARTESIAN_POINT('Origin',(3.,0.,3.9));
#7315=CARTESIAN_POINT('',(3.,-8.38883057415937E-17,4.585));
#7316=CARTESIAN_POINT('Origin',(3.,0.,3.9));
#7317=CARTESIAN_POINT('',(4.5,-8.38883057415937E-17,4.585));
#7318=CARTESIAN_POINT('',(3.,-8.38883057415937E-17,4.585));
#7319=CARTESIAN_POINT('',(4.44755831889813,0.685,3.9));
#7320=CARTESIAN_POINT('Ctrl Pts',(4.44755831889813,0.685,3.9));
#7321=CARTESIAN_POINT('Ctrl Pts',(4.44755831889813,0.685,3.81384504423947));
#7322=CARTESIAN_POINT('Ctrl Pts',(4.4503204226392,0.667754444280465,3.72204054828539));
#7323=CARTESIAN_POINT('Ctrl Pts',(4.46025507446226,0.59780642365717,3.55331129385551));
#7324=CARTESIAN_POINT('Ctrl Pts',(4.46727957365527,0.545111157186078,3.47637486696051));
#7325=CARTESIAN_POINT('Ctrl Pts',(4.48043230270009,0.42362625704472,3.35488996681915));
#7326=CARTESIAN_POINT('Ctrl Pts',(4.48742111878839,0.346689345476453,3.30219381864495));
#7327=CARTESIAN_POINT('Ctrl Pts',(4.49727390705164,0.177958434129502,3.23224515660969));
#7328=CARTESIAN_POINT('Ctrl Pts',(4.5,0.086153361525777,3.215));
#7329=CARTESIAN_POINT('Ctrl Pts',(4.5,-0.0861533615257769,3.215));
#7330=CARTESIAN_POINT('Ctrl Pts',(4.49727390705164,-0.177958434129502,3.23224515660969));
#7331=CARTESIAN_POINT('Ctrl Pts',(4.48742111878839,-0.346689345476453,3.30219381864495));
#7332=CARTESIAN_POINT('Ctrl Pts',(4.48043230270009,-0.42362625704472,3.35488996681915));
#7333=CARTESIAN_POINT('Ctrl Pts',(4.46727957365527,-0.545111157186078,3.47637486696051));
#7334=CARTESIAN_POINT('Ctrl Pts',(4.46025507446226,-0.597806423657171,3.55331129385551));
#7335=CARTESIAN_POINT('Ctrl Pts',(4.4503204226392,-0.667754444280465,3.72204054828539));
#7336=CARTESIAN_POINT('Ctrl Pts',(4.44755831889813,-0.685,3.81384504423947));
#7337=CARTESIAN_POINT('Ctrl Pts',(4.44755831889813,-0.685,3.98615495576053));
#7338=CARTESIAN_POINT('Ctrl Pts',(4.4503204226392,-0.667754444280465,4.0779594517146));
#7339=CARTESIAN_POINT('Ctrl Pts',(4.46025507446226,-0.597806423657171,4.24668870614449));
#7340=CARTESIAN_POINT('Ctrl Pts',(4.46727957365527,-0.545111157186078,4.32362513303949));
#7341=CARTESIAN_POINT('Ctrl Pts',(4.48043230270009,-0.42362625704472,4.44511003318085));
#7342=CARTESIAN_POINT('Ctrl Pts',(4.48742111878839,-0.346689345476454,4.49780618135505));
#7343=CARTESIAN_POINT('Ctrl Pts',(4.49727390705164,-0.177958434129502,4.56775484339031));
#7344=CARTESIAN_POINT('Ctrl Pts',(4.5,-0.0861533615257772,4.585));
#7345=CARTESIAN_POINT('Ctrl Pts',(4.5,-1.38777878078145E-16,4.585));
#7346=CARTESIAN_POINT('Ctrl Pts',(4.5,-8.32667268468867E-17,4.585));
#7347=CARTESIAN_POINT('Ctrl Pts',(4.5,0.086153361525777,4.585));
#7348=CARTESIAN_POINT('Ctrl Pts',(4.49727390705164,0.177958434129502,4.56775484339031));
#7349=CARTESIAN_POINT('Ctrl Pts',(4.48742111878839,0.346689345476453,4.49780618135505));
#7350=CARTESIAN_POINT('Ctrl Pts',(4.48043230270009,0.42362625704472,4.44511003318085));
#7351=CARTESIAN_POINT('Ctrl Pts',(4.46727957365527,0.545111157186078,4.32362513303949));
#7352=CARTESIAN_POINT('Ctrl Pts',(4.46025507446226,0.597806423657171,4.24668870614449));
#7353=CARTESIAN_POINT('Ctrl Pts',(4.4503204226392,0.667754444280465,4.07795945171461));
#7354=CARTESIAN_POINT('Ctrl Pts',(4.44755831889813,0.685,3.98615495576053));
#7355=CARTESIAN_POINT('Ctrl Pts',(4.44755831889813,0.685,3.9));
#7356=CARTESIAN_POINT('Origin',(3.,0.,3.9));
#7357=CARTESIAN_POINT('Origin',(-1.8,0.,2.4));
#7358=CARTESIAN_POINT('',(-1.7,-0.387298334620742,2.4));
#7359=CARTESIAN_POINT('',(-1.9,-0.387298334620742,2.4));
#7360=CARTESIAN_POINT('',(-3.1,-0.387298334620742,2.4));
#7361=CARTESIAN_POINT('Origin',(-1.8,0.,2.4));
#7362=CARTESIAN_POINT('Origin',(-1.8,0.,2.4));
#7363=CARTESIAN_POINT('',(-1.9,0.387298334620742,2.4));
#7364=CARTESIAN_POINT('',(-1.7,0.387298334620742,2.4));
#7365=CARTESIAN_POINT('',(-3.1,0.387298334620742,2.4));
#7366=CARTESIAN_POINT('Origin',(-1.8,0.,2.4));
#7367=CARTESIAN_POINT('Origin',(-1.8,0.,2.4));
#7368=CARTESIAN_POINT('',(-1.6,0.346410161513776,2.4));
#7369=CARTESIAN_POINT('',(-1.6,-0.346410161513776,2.4));
#7370=CARTESIAN_POINT('',(-1.6,0.,2.4));
#7371=CARTESIAN_POINT('Origin',(-1.8,0.,2.4));
#7372=CARTESIAN_POINT('Origin',(-1.8,0.,0.9));
#7373=CARTESIAN_POINT('',(-1.8,-0.4,2.3));
#7374=CARTESIAN_POINT('Origin',(-1.8,0.,2.3));
#7375=CARTESIAN_POINT('Origin',(-1.8,0.,2.3));
#7376=CARTESIAN_POINT('Origin',(-1.8,0.,0.9));
#7377=CARTESIAN_POINT('',(-1.8,0.4,2.3));
#7378=CARTESIAN_POINT('Origin',(-1.8,0.,2.3));
#7379=CARTESIAN_POINT('Origin',(-1.8,0.,2.3));
#7380=CARTESIAN_POINT('Origin',(-1.8,0.,0.9));
#7381=CARTESIAN_POINT('',(-2.2,-4.89858719658941E-17,1.4));
#7382=CARTESIAN_POINT('Origin',(-1.8,0.,1.4));
#7383=CARTESIAN_POINT('',(-2.2,-4.89858719658941E-17,1.9));
#7384=CARTESIAN_POINT('',(-2.2,-4.89858719658941E-17,0.9));
#7385=CARTESIAN_POINT('Origin',(-1.8,0.,2.3));
#7386=CARTESIAN_POINT('',(-1.6,-0.346410161513776,2.1));
#7387=CARTESIAN_POINT('Origin',(-1.8,0.,2.3));
#7388=CARTESIAN_POINT('',(-1.6,-0.346410161513776,0.9));
#7389=CARTESIAN_POINT('',(-1.6,0.346410161513776,2.1));
#7390=CARTESIAN_POINT('',(-1.6,0.346410161513776,0.9));
#7391=CARTESIAN_POINT('Origin',(-1.8,0.,2.3));
#7392=CARTESIAN_POINT('Origin',(-1.8,0.,2.3));
#7393=CARTESIAN_POINT('Origin',(-1.6,0.,2.3));
#7394=CARTESIAN_POINT('',(-1.6,-4.89858719658941E-17,2.7));
#7395=CARTESIAN_POINT('Origin',(-1.6,0.,2.3));
#7396=CARTESIAN_POINT('Origin',(-1.6,0.,2.3));
#7397=CARTESIAN_POINT('Origin',(-3.1,0.,2.3));
#7398=CARTESIAN_POINT('',(-3.,-4.89858719658941E-17,2.7));
#7399=CARTESIAN_POINT('Origin',(-3.,0.,2.3));
#7400=CARTESIAN_POINT('',(-3.1,-4.89858719658941E-17,2.7));
#7401=CARTESIAN_POINT('Origin',(-4.6,0.,2.3));
#7402=CARTESIAN_POINT('',(-4.44755831889813,0.685,2.3));
#7403=CARTESIAN_POINT('',(-4.5,-8.38883057415937E-17,2.985));
#7404=CARTESIAN_POINT('Ctrl Pts',(-4.44755831889813,0.685,2.3));
#7405=CARTESIAN_POINT('Ctrl Pts',(-4.44755831889813,0.685,2.38615495576053));
#7406=CARTESIAN_POINT('Ctrl Pts',(-4.4503204226392,0.667754444280465,2.47795945171461));
#7407=CARTESIAN_POINT('Ctrl Pts',(-4.46025507446226,0.597806423657171,2.64668870614449));
#7408=CARTESIAN_POINT('Ctrl Pts',(-4.46727957365527,0.545111157186078,2.72362513303949));
#7409=CARTESIAN_POINT('Ctrl Pts',(-4.48043230270009,0.42362625704472,2.84511003318085));
#7410=CARTESIAN_POINT('Ctrl Pts',(-4.48742111878839,0.346689345476453,2.89780618135505));
#7411=CARTESIAN_POINT('Ctrl Pts',(-4.49727390705164,0.177958434129502,2.96775484339031));
#7412=CARTESIAN_POINT('Ctrl Pts',(-4.5,0.0861533615257772,2.985));
#7413=CARTESIAN_POINT('Ctrl Pts',(-4.5,1.11022302462516E-16,2.985));
#7414=CARTESIAN_POINT('',(-4.5,-3.58812256655041E-16,1.615));
#7415=CARTESIAN_POINT('Ctrl Pts',(-4.5,-1.66533453693773E-16,1.615));
#7416=CARTESIAN_POINT('Ctrl Pts',(-4.5,0.0861533615257768,1.615));
#7417=CARTESIAN_POINT('Ctrl Pts',(-4.49727390705164,0.177958434129502,1.63224515660969));
#7418=CARTESIAN_POINT('Ctrl Pts',(-4.48742111878839,0.346689345476453,1.70219381864495));
#7419=CARTESIAN_POINT('Ctrl Pts',(-4.48043230270009,0.42362625704472,1.75488996681915));
#7420=CARTESIAN_POINT('Ctrl Pts',(-4.46727957365527,0.545111157186078,1.87637486696051));
#7421=CARTESIAN_POINT('Ctrl Pts',(-4.46025507446226,0.597806423657171,1.95331129385551));
#7422=CARTESIAN_POINT('Ctrl Pts',(-4.4503204226392,0.667754444280465,2.12204054828539));
#7423=CARTESIAN_POINT('Ctrl Pts',(-4.44755831889813,0.685,2.21384504423947));
#7424=CARTESIAN_POINT('Ctrl Pts',(-4.44755831889813,0.685,2.3));
#7425=CARTESIAN_POINT('Ctrl Pts',(-4.5,1.11022302462516E-16,2.985));
#7426=CARTESIAN_POINT('Ctrl Pts',(-4.5,-0.0861533615257769,2.985));
#7427=CARTESIAN_POINT('Ctrl Pts',(-4.49727390705164,-0.177958434129502,
2.96775484339031));
#7428=CARTESIAN_POINT('Ctrl Pts',(-4.48742111878839,-0.346689345476453,
2.89780618135505));
#7429=CARTESIAN_POINT('Ctrl Pts',(-4.48043230270009,-0.42362625704472,2.84511003318085));
#7430=CARTESIAN_POINT('Ctrl Pts',(-4.46727957365527,-0.545111157186078,
2.72362513303949));
#7431=CARTESIAN_POINT('Ctrl Pts',(-4.46025507446226,-0.597806423657171,
2.64668870614449));
#7432=CARTESIAN_POINT('Ctrl Pts',(-4.4503204226392,-0.667754444280465,2.47795945171461));
#7433=CARTESIAN_POINT('Ctrl Pts',(-4.44755831889813,-0.685,2.38615495576053));
#7434=CARTESIAN_POINT('Ctrl Pts',(-4.44755831889813,-0.685,2.21384504423947));
#7435=CARTESIAN_POINT('Ctrl Pts',(-4.4503204226392,-0.667754444280465,2.12204054828539));
#7436=CARTESIAN_POINT('Ctrl Pts',(-4.46025507446226,-0.597806423657171,
1.95331129385551));
#7437=CARTESIAN_POINT('Ctrl Pts',(-4.46727957365527,-0.545111157186078,
1.87637486696051));
#7438=CARTESIAN_POINT('Ctrl Pts',(-4.48043230270009,-0.42362625704472,1.75488996681915));
#7439=CARTESIAN_POINT('Ctrl Pts',(-4.48742111878839,-0.346689345476453,
1.70219381864495));
#7440=CARTESIAN_POINT('Ctrl Pts',(-4.49727390705164,-0.177958434129502,
1.63224515660969));
#7441=CARTESIAN_POINT('Ctrl Pts',(-4.5,-0.0861533615257771,1.615));
#7442=CARTESIAN_POINT('Ctrl Pts',(-4.5,-1.38777878078145E-16,1.615));
#7443=CARTESIAN_POINT('',(-3.,-8.38883057415937E-17,2.985));
#7444=CARTESIAN_POINT('',(-4.6,-8.38883057415937E-17,2.985));
#7445=CARTESIAN_POINT('Origin',(-3.,0.,2.3));
#7446=CARTESIAN_POINT('Origin',(-3.,0.,2.3));
#7447=CARTESIAN_POINT('Origin',(0.,0.,0.76));
#7448=CARTESIAN_POINT('',(-0.89,-1.08993565124114E-16,0.76));
#7449=CARTESIAN_POINT('Origin',(0.,0.,0.76));
#7450=CARTESIAN_POINT('',(-0.89,-1.08993565124114E-16,1.04));
#7451=CARTESIAN_POINT('',(-0.89,-1.08993565124114E-16,0.76));
#7452=CARTESIAN_POINT('Origin',(0.,0.,1.04));
#7453=CARTESIAN_POINT('Origin',(0.,0.,1.04));
#7454=CARTESIAN_POINT('',(-0.6185,7.57444045272638E-17,1.04));
#7455=CARTESIAN_POINT('Origin',(0.,0.,1.04));
#7456=CARTESIAN_POINT('Origin',(0.,0.,0.76));
#7457=CARTESIAN_POINT('',(-0.6185,-7.57444045272638E-17,0.76));
#7458=CARTESIAN_POINT('Origin',(0.,0.,0.76));
#7459=CARTESIAN_POINT('Origin',(0.,0.,0.4));
#7460=CARTESIAN_POINT('',(-0.6185,-7.57444045272638E-17,0.5));
#7461=CARTESIAN_POINT('Origin',(0.,0.,0.5));
#7462=CARTESIAN_POINT('',(-0.6185,-7.57444045272638E-17,0.4));
#7463=CARTESIAN_POINT('Origin',(0.,0.,0.4));
#7464=CARTESIAN_POINT('',(-0.6185,-7.57444045272638E-17,1.5));
#7465=CARTESIAN_POINT('',(-0.6185,-7.57444045272638E-17,0.4));
#7466=CARTESIAN_POINT('Origin',(0.,0.,1.5));
#7467=CARTESIAN_POINT('Origin',(0.,0.,0.5));
#7468=CARTESIAN_POINT('',(-1.1,-1.34711147906209E-16,1.4));
#7469=CARTESIAN_POINT('Origin',(0.,0.,1.4));
#7470=CARTESIAN_POINT('',(-1.1,-1.34711147906209E-16,0.5));
#7471=CARTESIAN_POINT('',(-1.1,-1.34711147906209E-16,0.5));
#7472=CARTESIAN_POINT('Origin',(0.,0.,0.5));
#7473=CARTESIAN_POINT('Origin',(0.,0.,1.5));
#7474=CARTESIAN_POINT('',(-0.8,9.79717439317883E-17,1.5));
#7475=CARTESIAN_POINT('Origin',(0.,0.,1.5));
#7476=CARTESIAN_POINT('Origin',(0.,0.,0.5));
#7477=CARTESIAN_POINT('Origin',(0.,0.,2.3));
#7478=CARTESIAN_POINT('',(-0.6,-7.34788079488412E-17,2.4));
#7479=CARTESIAN_POINT('Origin',(0.,0.,2.4));
#7480=CARTESIAN_POINT('',(-0.6,7.34788079488412E-17,3.2));
#7481=CARTESIAN_POINT('',(-0.6,-7.34788079488412E-17,2.3));
#7482=CARTESIAN_POINT('Origin',(0.,0.,3.2));
#7483=CARTESIAN_POINT('Origin',(0.,0.,1.4));
#7484=CARTESIAN_POINT('',(-0.8,-9.79717439317883E-17,2.4));
#7485=CARTESIAN_POINT('',(-0.8,-9.79717439317883E-17,1.4));
#7486=CARTESIAN_POINT('Origin',(0.,0.,2.4));
#7487=CARTESIAN_POINT('Origin',(0.,0.,2.4));
#7488=CARTESIAN_POINT('Origin',(0.,0.,3.2));
#7489=CARTESIAN_POINT('',(-2.5,-3.06161699786838E-16,3.2));
#7490=CARTESIAN_POINT('Origin',(0.,0.,3.2));
#7491=CARTESIAN_POINT('',(-2.5,3.06161699786838E-16,5.));
#7492=CARTESIAN_POINT('',(-2.5,-3.06161699786838E-16,3.2));
#7493=CARTESIAN_POINT('Origin',(0.,0.,5.));
#7494=CARTESIAN_POINT('Origin',(0.,0.,3.2));
#7495=CARTESIAN_POINT('Origin',(0.,0.,0.9));
#7496=CARTESIAN_POINT('',(-3.31,-4.05358090517774E-16,1.));
#7497=CARTESIAN_POINT('Origin',(0.,0.,1.));
#7498=CARTESIAN_POINT('',(-3.31,-4.05358090517774E-16,0.9));
#7499=CARTESIAN_POINT('Origin',(0.,0.,1.4));
#7500=CARTESIAN_POINT('Origin',(0.,0.,1.));
#7501=CARTESIAN_POINT('',(-4.5,-5.51091059616309E-16,5.));
#7502=CARTESIAN_POINT('Origin',(0.,0.,5.));
#7503=CARTESIAN_POINT('',(-4.5,-5.51091059616309E-16,1.));
#7504=CARTESIAN_POINT('',(-4.5,-5.51091059616309E-16,1.));
#7505=CARTESIAN_POINT('',(-4.5,-5.51091059616309E-16,1.));
#7506=CARTESIAN_POINT('Origin',(0.,0.,1.));
#7507=CARTESIAN_POINT('Origin',(0.,0.,5.));
#7508=CARTESIAN_POINT('Origin',(0.,0.,1.));
#7509=CARTESIAN_POINT('',(0.,0.,0.));
#7510=CARTESIAN_POINT('Origin',(0.,0.,1.4));
#7511=CARTESIAN_POINT('',(-2.25,-2.75545529808154E-16,1.4));
#7512=CARTESIAN_POINT('Origin',(-2.35,-2.87791997799628E-16,1.4));
#7513=CARTESIAN_POINT('Origin',(0.,0.,1.4));
#7514=CARTESIAN_POINT('',(0.,0.,0.));
#7515=CARTESIAN_POINT('Origin',(0.,-1.3,-2.5));
#7516=CARTESIAN_POINT('',(-0.05,-1.19895788082818,-2.5));
#7517=CARTESIAN_POINT('Ctrl Pts',(-0.05,-1.19895788082818,-2.5));
#7518=CARTESIAN_POINT('Ctrl Pts',(-0.05,-1.19895788082818,-2.49372110852169));
#7519=CARTESIAN_POINT('Ctrl Pts',(-0.0487450133099081,-1.19901227819454,
-2.48702419537593));
#7520=CARTESIAN_POINT('Ctrl Pts',(-0.0436421041657014,-1.19920885850753,
-2.47470544370928));
#7521=CARTESIAN_POINT('Ctrl Pts',(-0.0397942217705328,-1.1993482149535,
-2.46908354365188));
#7522=CARTESIAN_POINT('Ctrl Pts',(-0.0309164568000038,-1.19960989221221,
-2.46020577868135));
#7523=CARTESIAN_POINT('Ctrl Pts',(-0.0252945565319674,-1.19974919586288,
-2.45635789595805));
#7524=CARTESIAN_POINT('Ctrl Pts',(-0.0129758042228731,-1.19994565546462,
-2.45125498650009));
#7525=CARTESIAN_POINT('Ctrl Pts',(-0.00627889083911039,-1.2,-2.45));
#7526=CARTESIAN_POINT('Ctrl Pts',(0.00627889083911038,-1.2,-2.45));
#7527=CARTESIAN_POINT('Ctrl Pts',(0.012975804222873,-1.19994565546462,-2.45125498650009));
#7528=CARTESIAN_POINT('Ctrl Pts',(0.0252945565319674,-1.19974919586288,
-2.45635789595805));
#7529=CARTESIAN_POINT('Ctrl Pts',(0.0309164568000038,-1.19960989221221,
-2.46020577868135));
#7530=CARTESIAN_POINT('Ctrl Pts',(0.0397942217705328,-1.1993482149535,-2.46908354365188));
#7531=CARTESIAN_POINT('Ctrl Pts',(0.0436421041657014,-1.19920885850753,
-2.47470544370928));
#7532=CARTESIAN_POINT('Ctrl Pts',(0.0487450133099081,-1.19901227819454,
-2.48702419537593));
#7533=CARTESIAN_POINT('Ctrl Pts',(0.05,-1.19895788082818,-2.49372110852169));
#7534=CARTESIAN_POINT('Ctrl Pts',(0.05,-1.19895788082818,-2.50627889147831));
#7535=CARTESIAN_POINT('Ctrl Pts',(0.0487450133099081,-1.19901227819454,
-2.51297580462407));
#7536=CARTESIAN_POINT('Ctrl Pts',(0.0436421041657014,-1.19920885850753,
-2.52529455629072));
#7537=CARTESIAN_POINT('Ctrl Pts',(0.0397942217705328,-1.1993482149535,-2.53091645634812));
#7538=CARTESIAN_POINT('Ctrl Pts',(0.0309164568000038,-1.19960989221221,
-2.53979422131865));
#7539=CARTESIAN_POINT('Ctrl Pts',(0.0252945565319675,-1.19974919586288,
-2.54364210404195));
#7540=CARTESIAN_POINT('Ctrl Pts',(0.0129758042228731,-1.19994565546462,
-2.54874501349991));
#7541=CARTESIAN_POINT('Ctrl Pts',(0.0062788908391104,-1.2,-2.55));
#7542=CARTESIAN_POINT('Ctrl Pts',(-0.00627889083911037,-1.2,-2.55));
#7543=CARTESIAN_POINT('Ctrl Pts',(-0.012975804222873,-1.19994565546462,
-2.54874501349991));
#7544=CARTESIAN_POINT('Ctrl Pts',(-0.0252945565319674,-1.19974919586288,
-2.54364210404195));
#7545=CARTESIAN_POINT('Ctrl Pts',(-0.0309164568000038,-1.19960989221221,
-2.53979422131865));
#7546=CARTESIAN_POINT('Ctrl Pts',(-0.0397942217705328,-1.1993482149535,
-2.53091645634812));
#7547=CARTESIAN_POINT('Ctrl Pts',(-0.0436421041657014,-1.19920885850753,
-2.52529455629072));
#7548=CARTESIAN_POINT('Ctrl Pts',(-0.0487450133099081,-1.19901227819454,
-2.51297580462407));
#7549=CARTESIAN_POINT('Ctrl Pts',(-0.05,-1.19895788082818,-2.50627889147831));
#7550=CARTESIAN_POINT('Ctrl Pts',(-0.05,-1.19895788082818,-2.5));
#7551=CARTESIAN_POINT('',(-0.05,-0.396862696659689,-2.5));
#7552=CARTESIAN_POINT('',(-0.05,-1.3,-2.5));
#7553=CARTESIAN_POINT('Ctrl Pts',(-0.05,-0.396862696659689,-2.5));
#7554=CARTESIAN_POINT('Ctrl Pts',(-0.05,-0.396862696659689,-2.50628520096426));
#7555=CARTESIAN_POINT('Ctrl Pts',(-0.0487425534891116,-0.397027412247524,
-2.51298480122901));
#7556=CARTESIAN_POINT('Ctrl Pts',(-0.0436378373878618,-0.397620851691571,
-2.52530179409386));
#7557=CARTESIAN_POINT('Ctrl Pts',(-0.0397909243921696,-0.398040841710914,
-2.53091975372649));
#7558=CARTESIAN_POINT('Ctrl Pts',(-0.0309197907817458,-0.398828027526425,
-2.53979088733691));
#7559=CARTESIAN_POINT('Ctrl Pts',(-0.0253018150396577,-0.399246581249293,
-2.5436378293633));
#7560=CARTESIAN_POINT('Ctrl Pts',(-0.0129847676279313,-0.399836729543542,
-2.5487425667586));
#7561=CARTESIAN_POINT('Ctrl Pts',(-0.00628514845714647,-0.4,-2.55));
#7562=CARTESIAN_POINT('Ctrl Pts',(0.00628514845714648,-0.4,-2.55));
#7563=CARTESIAN_POINT('Ctrl Pts',(0.012984767627931,-0.399836729543542,
-2.5487425667586));
#7564=CARTESIAN_POINT('Ctrl Pts',(0.0253018150396574,-0.399246581249293,
-2.5436378293633));
#7565=CARTESIAN_POINT('Ctrl Pts',(0.0309197907817458,-0.398828027526425,
-2.53979088733691));
#7566=CARTESIAN_POINT('Ctrl Pts',(0.0397909243921696,-0.398040841710914,
-2.53091975372649));
#7567=CARTESIAN_POINT('Ctrl Pts',(0.0436378373878616,-0.397620851691571,
-2.52530179409386));
#7568=CARTESIAN_POINT('Ctrl Pts',(0.0487425534891115,-0.397027412247524,
-2.51298480122901));
#7569=CARTESIAN_POINT('Ctrl Pts',(0.05,-0.396862696659689,-2.50628520096426));
#7570=CARTESIAN_POINT('Ctrl Pts',(0.05,-0.396862696659689,-2.49371479903574));
#7571=CARTESIAN_POINT('Ctrl Pts',(0.0487425534891116,-0.397027412247524,
-2.48701519877099));
#7572=CARTESIAN_POINT('Ctrl Pts',(0.0436378373878618,-0.397620851691571,
-2.47469820590614));
#7573=CARTESIAN_POINT('Ctrl Pts',(0.0397909243921696,-0.398040841710914,
-2.46908024627351));
#7574=CARTESIAN_POINT('Ctrl Pts',(0.0309197907817458,-0.398828027526425,
-2.46020911266309));
#7575=CARTESIAN_POINT('Ctrl Pts',(0.0253018150396577,-0.399246581249293,
-2.4563621706367));
#7576=CARTESIAN_POINT('Ctrl Pts',(0.0129847676279313,-0.399836729543542,
-2.4512574332414));
#7577=CARTESIAN_POINT('Ctrl Pts',(0.00628514845714648,-0.4,-2.45));
#7578=CARTESIAN_POINT('Ctrl Pts',(-0.00628514845714647,-0.4,-2.45));
#7579=CARTESIAN_POINT('Ctrl Pts',(-0.0129847676279313,-0.399836729543542,
-2.4512574332414));
#7580=CARTESIAN_POINT('Ctrl Pts',(-0.0253018150396577,-0.399246581249293,
-2.4563621706367));
#7581=CARTESIAN_POINT('Ctrl Pts',(-0.0309197907817458,-0.398828027526425,
-2.46020911266309));
#7582=CARTESIAN_POINT('Ctrl Pts',(-0.0397909243921696,-0.398040841710914,
-2.46908024627351));
#7583=CARTESIAN_POINT('Ctrl Pts',(-0.0436378373878618,-0.397620851691571,
-2.47469820590614));
#7584=CARTESIAN_POINT('Ctrl Pts',(-0.0487425534891116,-0.397027412247524,
-2.48701519877099));
#7585=CARTESIAN_POINT('Ctrl Pts',(-0.05,-0.396862696659689,-2.49371479903574));
#7586=CARTESIAN_POINT('Ctrl Pts',(-0.05,-0.396862696659689,-2.5));
#7587=CARTESIAN_POINT('Origin',(0.,-1.3,-2.5));
#7588=CARTESIAN_POINT('',(-0.05,0.396862696659689,-2.5));
#7589=CARTESIAN_POINT('Ctrl Pts',(-0.05,0.396862696659689,-2.5));
#7590=CARTESIAN_POINT('Ctrl Pts',(-0.05,0.396862696659689,-2.49371479903574));
#7591=CARTESIAN_POINT('Ctrl Pts',(-0.0487425534891116,0.397027412247524,
-2.48701519877099));
#7592=CARTESIAN_POINT('Ctrl Pts',(-0.0436378373878618,0.397620851691571,
-2.47469820590614));
#7593=CARTESIAN_POINT('Ctrl Pts',(-0.0397909243921696,0.398040841710914,
-2.46908024627351));
#7594=CARTESIAN_POINT('Ctrl Pts',(-0.0309197907817458,0.398828027526425,
-2.46020911266309));
#7595=CARTESIAN_POINT('Ctrl Pts',(-0.0253018150396577,0.399246581249293,
-2.4563621706367));
#7596=CARTESIAN_POINT('Ctrl Pts',(-0.0129847676279313,0.399836729543542,
-2.4512574332414));
#7597=CARTESIAN_POINT('Ctrl Pts',(-0.00628514845714647,0.4,-2.45));
#7598=CARTESIAN_POINT('Ctrl Pts',(0.00628514845714648,0.4,-2.45));
#7599=CARTESIAN_POINT('Ctrl Pts',(0.0129847676279313,0.399836729543542,
-2.4512574332414));
#7600=CARTESIAN_POINT('Ctrl Pts',(0.0253018150396577,0.399246581249293,
-2.4563621706367));
#7601=CARTESIAN_POINT('Ctrl Pts',(0.0309197907817458,0.398828027526425,
-2.46020911266309));
#7602=CARTESIAN_POINT('Ctrl Pts',(0.0397909243921696,0.398040841710914,
-2.46908024627351));
#7603=CARTESIAN_POINT('Ctrl Pts',(0.0436378373878621,0.397620851691571,
-2.47469820590614));
#7604=CARTESIAN_POINT('Ctrl Pts',(0.0487425534891117,0.397027412247524,
-2.48701519877099));
#7605=CARTESIAN_POINT('Ctrl Pts',(0.05,0.396862696659689,-2.49371479903574));
#7606=CARTESIAN_POINT('Ctrl Pts',(0.05,0.396862696659689,-2.50628520096426));
#7607=CARTESIAN_POINT('Ctrl Pts',(0.0487425534891116,0.397027412247524,
-2.51298480122901));
#7608=CARTESIAN_POINT('Ctrl Pts',(0.0436378373878618,0.397620851691571,
-2.52530179409386));
#7609=CARTESIAN_POINT('Ctrl Pts',(0.0397909243921696,0.398040841710914,
-2.53091975372649));
#7610=CARTESIAN_POINT('Ctrl Pts',(0.0309197907817458,0.398828027526425,
-2.53979088733691));
#7611=CARTESIAN_POINT('Ctrl Pts',(0.0253018150396574,0.399246581249293,
-2.5436378293633));
#7612=CARTESIAN_POINT('Ctrl Pts',(0.012984767627931,0.399836729543542,-2.5487425667586));
#7613=CARTESIAN_POINT('Ctrl Pts',(0.00628514845714648,0.4,-2.55));
#7614=CARTESIAN_POINT('Ctrl Pts',(-0.00628514845714647,0.4,-2.55));
#7615=CARTESIAN_POINT('Ctrl Pts',(-0.012984767627931,0.399836729543542,
-2.5487425667586));
#7616=CARTESIAN_POINT('Ctrl Pts',(-0.0253018150396574,0.399246581249293,
-2.5436378293633));
#7617=CARTESIAN_POINT('Ctrl Pts',(-0.0309197907817458,0.398828027526425,
-2.53979088733691));
#7618=CARTESIAN_POINT('Ctrl Pts',(-0.0397909243921696,0.398040841710914,
-2.53091975372649));
#7619=CARTESIAN_POINT('Ctrl Pts',(-0.0436378373878618,0.397620851691571,
-2.52530179409386));
#7620=CARTESIAN_POINT('Ctrl Pts',(-0.0487425534891116,0.397027412247524,
-2.51298480122901));
#7621=CARTESIAN_POINT('Ctrl Pts',(-0.05,0.396862696659689,-2.50628520096426));
#7622=CARTESIAN_POINT('Ctrl Pts',(-0.05,0.396862696659689,-2.5));
#7623=CARTESIAN_POINT('',(-0.05,1.19895788082818,-2.5));
#7624=CARTESIAN_POINT('',(-0.05,-1.3,-2.5));
#7625=CARTESIAN_POINT('Ctrl Pts',(-0.05,1.19895788082818,-2.5));
#7626=CARTESIAN_POINT('Ctrl Pts',(-0.05,1.19895788082818,-2.50627889147831));
#7627=CARTESIAN_POINT('Ctrl Pts',(-0.0487450133099081,1.19901227819454,
-2.51297580462407));
#7628=CARTESIAN_POINT('Ctrl Pts',(-0.0436421041657014,1.19920885850753,
-2.52529455629072));
#7629=CARTESIAN_POINT('Ctrl Pts',(-0.0397942217705328,1.1993482149535,-2.53091645634812));
#7630=CARTESIAN_POINT('Ctrl Pts',(-0.0309164568000038,1.19960989221221,
-2.53979422131865));
#7631=CARTESIAN_POINT('Ctrl Pts',(-0.0252945565319674,1.19974919586288,
-2.54364210404195));
#7632=CARTESIAN_POINT('Ctrl Pts',(-0.012975804222873,1.19994565546462,-2.54874501349991));
#7633=CARTESIAN_POINT('Ctrl Pts',(-0.00627889083911037,1.2,-2.55));
#7634=CARTESIAN_POINT('Ctrl Pts',(0.0062788908391104,1.2,-2.55));
#7635=CARTESIAN_POINT('Ctrl Pts',(0.0129758042228731,1.19994565546462,-2.54874501349991));
#7636=CARTESIAN_POINT('Ctrl Pts',(0.0252945565319675,1.19974919586288,-2.54364210404195));
#7637=CARTESIAN_POINT('Ctrl Pts',(0.0309164568000038,1.19960989221221,-2.53979422131865));
#7638=CARTESIAN_POINT('Ctrl Pts',(0.0397942217705328,1.1993482149535,-2.53091645634812));
#7639=CARTESIAN_POINT('Ctrl Pts',(0.0436421041657014,1.19920885850753,-2.52529455629072));
#7640=CARTESIAN_POINT('Ctrl Pts',(0.0487450133099081,1.19901227819454,-2.51297580462407));
#7641=CARTESIAN_POINT('Ctrl Pts',(0.05,1.19895788082818,-2.50627889147831));
#7642=CARTESIAN_POINT('Ctrl Pts',(0.05,1.19895788082818,-2.49372110852169));
#7643=CARTESIAN_POINT('Ctrl Pts',(0.0487450133099081,1.19901227819454,-2.48702419537593));
#7644=CARTESIAN_POINT('Ctrl Pts',(0.0436421041657014,1.19920885850753,-2.47470544370928));
#7645=CARTESIAN_POINT('Ctrl Pts',(0.0397942217705328,1.1993482149535,-2.46908354365188));
#7646=CARTESIAN_POINT('Ctrl Pts',(0.0309164568000038,1.19960989221221,-2.46020577868135));
#7647=CARTESIAN_POINT('Ctrl Pts',(0.0252945565319674,1.19974919586288,-2.45635789595805));
#7648=CARTESIAN_POINT('Ctrl Pts',(0.012975804222873,1.19994565546462,-2.45125498650009));
#7649=CARTESIAN_POINT('Ctrl Pts',(0.00627889083911038,1.2,-2.45));
#7650=CARTESIAN_POINT('Ctrl Pts',(-0.00627889083911039,1.2,-2.45));
#7651=CARTESIAN_POINT('Ctrl Pts',(-0.0129758042228731,1.19994565546462,
-2.45125498650009));
#7652=CARTESIAN_POINT('Ctrl Pts',(-0.0252945565319674,1.19974919586288,
-2.45635789595805));
#7653=CARTESIAN_POINT('Ctrl Pts',(-0.0309164568000038,1.19960989221221,
-2.46020577868135));
#7654=CARTESIAN_POINT('Ctrl Pts',(-0.0397942217705328,1.1993482149535,-2.46908354365188));
#7655=CARTESIAN_POINT('Ctrl Pts',(-0.0436421041657014,1.19920885850753,
-2.47470544370928));
#7656=CARTESIAN_POINT('Ctrl Pts',(-0.0487450133099081,1.19901227819454,
-2.48702419537593));
#7657=CARTESIAN_POINT('Ctrl Pts',(-0.05,1.19895788082818,-2.49372110852169));
#7658=CARTESIAN_POINT('Ctrl Pts',(-0.05,1.19895788082818,-2.5));
#7659=CARTESIAN_POINT('Origin',(0.,-1.3,-1.5));
#7660=CARTESIAN_POINT('',(-0.05,-1.19895788082818,-1.5));
#7661=CARTESIAN_POINT('Ctrl Pts',(-0.05,-1.19895788082818,-1.5));
#7662=CARTESIAN_POINT('Ctrl Pts',(-0.05,-1.19895788082818,-1.49372110852169));
#7663=CARTESIAN_POINT('Ctrl Pts',(-0.0487450133099081,-1.19901227819454,
-1.48702419537594));
#7664=CARTESIAN_POINT('Ctrl Pts',(-0.0436421041657014,-1.19920885850753,
-1.47470544370928));
#7665=CARTESIAN_POINT('Ctrl Pts',(-0.0397942217705328,-1.1993482149535,
-1.46908354365188));
#7666=CARTESIAN_POINT('Ctrl Pts',(-0.0309164568000038,-1.19960989221221,
-1.46020577868135));
#7667=CARTESIAN_POINT('Ctrl Pts',(-0.0252945565319674,-1.19974919586288,
-1.45635789595805));
#7668=CARTESIAN_POINT('Ctrl Pts',(-0.012975804222873,-1.19994565546462,
-1.45125498650009));
#7669=CARTESIAN_POINT('Ctrl Pts',(-0.00627889083911039,-1.2,-1.45));
#7670=CARTESIAN_POINT('Ctrl Pts',(0.00627889083911038,-1.2,-1.45));
#7671=CARTESIAN_POINT('Ctrl Pts',(0.012975804222873,-1.19994565546462,-1.45125498650009));
#7672=CARTESIAN_POINT('Ctrl Pts',(0.0252945565319674,-1.19974919586288,
-1.45635789595805));
#7673=CARTESIAN_POINT('Ctrl Pts',(0.0309164568000038,-1.19960989221221,
-1.46020577868135));
#7674=CARTESIAN_POINT('Ctrl Pts',(0.0397942217705328,-1.1993482149535,-1.46908354365188));
#7675=CARTESIAN_POINT('Ctrl Pts',(0.0436421041657014,-1.19920885850753,
-1.47470544370928));
#7676=CARTESIAN_POINT('Ctrl Pts',(0.0487450133099081,-1.19901227819454,
-1.48702419537594));
#7677=CARTESIAN_POINT('Ctrl Pts',(0.05,-1.19895788082818,-1.49372110852169));
#7678=CARTESIAN_POINT('Ctrl Pts',(0.05,-1.19895788082818,-1.50627889147831));
#7679=CARTESIAN_POINT('Ctrl Pts',(0.0487450133099081,-1.19901227819454,
-1.51297580462406));
#7680=CARTESIAN_POINT('Ctrl Pts',(0.0436421041657014,-1.19920885850753,
-1.52529455629072));
#7681=CARTESIAN_POINT('Ctrl Pts',(0.0397942217705328,-1.1993482149535,-1.53091645634812));
#7682=CARTESIAN_POINT('Ctrl Pts',(0.0309164568000038,-1.19960989221221,
-1.53979422131865));
#7683=CARTESIAN_POINT('Ctrl Pts',(0.0252945565319674,-1.19974919586288,
-1.54364210404195));
#7684=CARTESIAN_POINT('Ctrl Pts',(0.0129758042228729,-1.19994565546462,
-1.54874501349991));
#7685=CARTESIAN_POINT('Ctrl Pts',(0.00627889083911041,-1.2,-1.55));
#7686=CARTESIAN_POINT('Ctrl Pts',(-0.00627889083911036,-1.2,-1.55));
#7687=CARTESIAN_POINT('Ctrl Pts',(-0.0129758042228728,-1.19994565546462,
-1.54874501349991));
#7688=CARTESIAN_POINT('Ctrl Pts',(-0.0252945565319673,-1.19974919586288,
-1.54364210404195));
#7689=CARTESIAN_POINT('Ctrl Pts',(-0.0309164568000037,-1.19960989221221,
-1.53979422131865));
#7690=CARTESIAN_POINT('Ctrl Pts',(-0.0397942217705328,-1.1993482149535,
-1.53091645634812));
#7691=CARTESIAN_POINT('Ctrl Pts',(-0.0436421041657014,-1.19920885850753,
-1.52529455629072));
#7692=CARTESIAN_POINT('Ctrl Pts',(-0.0487450133099081,-1.19901227819454,
-1.51297580462406));
#7693=CARTESIAN_POINT('Ctrl Pts',(-0.05,-1.19895788082818,-1.50627889147831));
#7694=CARTESIAN_POINT('Ctrl Pts',(-0.05,-1.19895788082818,-1.5));
#7695=CARTESIAN_POINT('',(-0.05,-0.396862696659689,-1.5));
#7696=CARTESIAN_POINT('',(-0.05,-1.3,-1.5));
#7697=CARTESIAN_POINT('Ctrl Pts',(-0.05,-0.396862696659689,-1.5));
#7698=CARTESIAN_POINT('Ctrl Pts',(-0.05,-0.396862696659689,-1.50628520096425));
#7699=CARTESIAN_POINT('Ctrl Pts',(-0.0487425534891115,-0.397027412247524,
-1.51298480122901));
#7700=CARTESIAN_POINT('Ctrl Pts',(-0.0436378373878619,-0.397620851691571,
-1.52530179409386));
#7701=CARTESIAN_POINT('Ctrl Pts',(-0.0397909243921696,-0.398040841710914,
-1.53091975372649));
#7702=CARTESIAN_POINT('Ctrl Pts',(-0.0309197907817458,-0.398828027526425,
-1.53979088733691));
#7703=CARTESIAN_POINT('Ctrl Pts',(-0.0253018150396575,-0.399246581249293,
-1.5436378293633));
#7704=CARTESIAN_POINT('Ctrl Pts',(-0.0129847676279312,-0.399836729543542,
-1.54874256675859));
#7705=CARTESIAN_POINT('Ctrl Pts',(-0.00628514845714648,-0.4,-1.55));
#7706=CARTESIAN_POINT('Ctrl Pts',(0.00628514845714648,-0.4,-1.55));
#7707=CARTESIAN_POINT('Ctrl Pts',(0.012984767627931,-0.399836729543542,
-1.54874256675859));
#7708=CARTESIAN_POINT('Ctrl Pts',(0.0253018150396574,-0.399246581249293,
-1.5436378293633));
#7709=CARTESIAN_POINT('Ctrl Pts',(0.0309197907817458,-0.398828027526425,
-1.53979088733691));
#7710=CARTESIAN_POINT('Ctrl Pts',(0.0397909243921696,-0.398040841710914,
-1.53091975372649));
#7711=CARTESIAN_POINT('Ctrl Pts',(0.0436378373878617,-0.397620851691571,
-1.52530179409386));
#7712=CARTESIAN_POINT('Ctrl Pts',(0.0487425534891115,-0.397027412247524,
-1.51298480122901));
#7713=CARTESIAN_POINT('Ctrl Pts',(0.05,-0.396862696659689,-1.50628520096426));
#7714=CARTESIAN_POINT('Ctrl Pts',(0.05,-0.396862696659689,-1.49371479903575));
#7715=CARTESIAN_POINT('Ctrl Pts',(0.0487425534891115,-0.397027412247524,
-1.48701519877099));
#7716=CARTESIAN_POINT('Ctrl Pts',(0.0436378373878619,-0.397620851691571,
-1.47469820590614));
#7717=CARTESIAN_POINT('Ctrl Pts',(0.0397909243921696,-0.398040841710914,
-1.46908024627351));
#7718=CARTESIAN_POINT('Ctrl Pts',(0.0309197907817458,-0.398828027526425,
-1.46020911266309));
#7719=CARTESIAN_POINT('Ctrl Pts',(0.0253018150396577,-0.399246581249293,
-1.4563621706367));
#7720=CARTESIAN_POINT('Ctrl Pts',(0.0129847676279313,-0.399836729543542,
-1.45125743324141));
#7721=CARTESIAN_POINT('Ctrl Pts',(0.00628514845714648,-0.4,-1.45));
#7722=CARTESIAN_POINT('Ctrl Pts',(-0.00628514845714647,-0.4,-1.45));
#7723=CARTESIAN_POINT('Ctrl Pts',(-0.0129847676279313,-0.399836729543542,
-1.45125743324141));
#7724=CARTESIAN_POINT('Ctrl Pts',(-0.0253018150396577,-0.399246581249293,
-1.4563621706367));
#7725=CARTESIAN_POINT('Ctrl Pts',(-0.0309197907817458,-0.398828027526425,
-1.46020911266309));
#7726=CARTESIAN_POINT('Ctrl Pts',(-0.0397909243921696,-0.398040841710914,
-1.46908024627351));
#7727=CARTESIAN_POINT('Ctrl Pts',(-0.0436378373878619,-0.397620851691571,
-1.47469820590614));
#7728=CARTESIAN_POINT('Ctrl Pts',(-0.0487425534891115,-0.397027412247524,
-1.48701519877099));
#7729=CARTESIAN_POINT('Ctrl Pts',(-0.05,-0.396862696659689,-1.49371479903575));
#7730=CARTESIAN_POINT('Ctrl Pts',(-0.05,-0.396862696659689,-1.5));
#7731=CARTESIAN_POINT('Origin',(0.,-1.3,-1.5));
#7732=CARTESIAN_POINT('',(-0.05,0.396862696659689,-1.5));
#7733=CARTESIAN_POINT('Ctrl Pts',(-0.05,0.396862696659689,-1.5));
#7734=CARTESIAN_POINT('Ctrl Pts',(-0.05,0.396862696659689,-1.49371479903575));
#7735=CARTESIAN_POINT('Ctrl Pts',(-0.0487425534891115,0.397027412247524,
-1.48701519877099));
#7736=CARTESIAN_POINT('Ctrl Pts',(-0.0436378373878619,0.397620851691571,
-1.47469820590614));
#7737=CARTESIAN_POINT('Ctrl Pts',(-0.0397909243921696,0.398040841710914,
-1.46908024627351));
#7738=CARTESIAN_POINT('Ctrl Pts',(-0.0309197907817458,0.398828027526425,
-1.46020911266309));
#7739=CARTESIAN_POINT('Ctrl Pts',(-0.0253018150396577,0.399246581249293,
-1.4563621706367));
#7740=CARTESIAN_POINT('Ctrl Pts',(-0.0129847676279313,0.399836729543542,
-1.4512574332414));
#7741=CARTESIAN_POINT('Ctrl Pts',(-0.00628514845714647,0.4,-1.45));
#7742=CARTESIAN_POINT('Ctrl Pts',(0.00628514845714648,0.4,-1.45));
#7743=CARTESIAN_POINT('Ctrl Pts',(0.0129847676279313,0.399836729543542,
-1.45125743324141));
#7744=CARTESIAN_POINT('Ctrl Pts',(0.0253018150396577,0.399246581249293,
-1.4563621706367));
#7745=CARTESIAN_POINT('Ctrl Pts',(0.0309197907817458,0.398828027526425,
-1.46020911266309));
#7746=CARTESIAN_POINT('Ctrl Pts',(0.0397909243921696,0.398040841710914,
-1.46908024627351));
#7747=CARTESIAN_POINT('Ctrl Pts',(0.0436378373878621,0.397620851691571,
-1.47469820590614));
#7748=CARTESIAN_POINT('Ctrl Pts',(0.0487425534891116,0.397027412247524,
-1.48701519877099));
#7749=CARTESIAN_POINT('Ctrl Pts',(0.05,0.396862696659689,-1.49371479903575));
#7750=CARTESIAN_POINT('Ctrl Pts',(0.05,0.396862696659689,-1.50628520096425));
#7751=CARTESIAN_POINT('Ctrl Pts',(0.0487425534891115,0.397027412247524,
-1.51298480122901));
#7752=CARTESIAN_POINT('Ctrl Pts',(0.0436378373878619,0.397620851691571,
-1.52530179409386));
#7753=CARTESIAN_POINT('Ctrl Pts',(0.0397909243921696,0.398040841710914,
-1.53091975372649));
#7754=CARTESIAN_POINT('Ctrl Pts',(0.0309197907817458,0.398828027526425,
-1.53979088733691));
#7755=CARTESIAN_POINT('Ctrl Pts',(0.0253018150396575,0.399246581249293,
-1.5436378293633));
#7756=CARTESIAN_POINT('Ctrl Pts',(0.0129847676279312,0.399836729543542,
-1.54874256675859));
#7757=CARTESIAN_POINT('Ctrl Pts',(0.00628514845714648,0.4,-1.55));
#7758=CARTESIAN_POINT('Ctrl Pts',(-0.00628514845714648,0.4,-1.55));
#7759=CARTESIAN_POINT('Ctrl Pts',(-0.0129847676279312,0.399836729543542,
-1.54874256675859));
#7760=CARTESIAN_POINT('Ctrl Pts',(-0.0253018150396575,0.399246581249293,
-1.5436378293633));
#7761=CARTESIAN_POINT('Ctrl Pts',(-0.0309197907817458,0.398828027526425,
-1.53979088733691));
#7762=CARTESIAN_POINT('Ctrl Pts',(-0.0397909243921696,0.398040841710914,
-1.53091975372648));
#7763=CARTESIAN_POINT('Ctrl Pts',(-0.043637837387862,0.397620851691571,
-1.52530179409386));
#7764=CARTESIAN_POINT('Ctrl Pts',(-0.0487425534891116,0.397027412247524,
-1.51298480122901));
#7765=CARTESIAN_POINT('Ctrl Pts',(-0.05,0.396862696659689,-1.50628520096425));
#7766=CARTESIAN_POINT('Ctrl Pts',(-0.05,0.396862696659689,-1.5));
#7767=CARTESIAN_POINT('',(-0.05,1.19895788082818,-1.5));
#7768=CARTESIAN_POINT('',(-0.05,-1.3,-1.5));
#7769=CARTESIAN_POINT('Ctrl Pts',(-0.05,1.19895788082818,-1.5));
#7770=CARTESIAN_POINT('Ctrl Pts',(-0.05,1.19895788082818,-1.50627889147831));
#7771=CARTESIAN_POINT('Ctrl Pts',(-0.0487450133099081,1.19901227819454,
-1.51297580462407));
#7772=CARTESIAN_POINT('Ctrl Pts',(-0.0436421041657012,1.19920885850753,
-1.52529455629072));
#7773=CARTESIAN_POINT('Ctrl Pts',(-0.0397942217705328,1.1993482149535,-1.53091645634812));
#7774=CARTESIAN_POINT('Ctrl Pts',(-0.0309164568000037,1.19960989221221,
-1.53979422131865));
#7775=CARTESIAN_POINT('Ctrl Pts',(-0.0252945565319673,1.19974919586288,
-1.54364210404195));
#7776=CARTESIAN_POINT('Ctrl Pts',(-0.0129758042228728,1.19994565546462,
-1.54874501349991));
#7777=CARTESIAN_POINT('Ctrl Pts',(-0.00627889083911036,1.2,-1.55));
#7778=CARTESIAN_POINT('Ctrl Pts',(0.00627889083911041,1.2,-1.55));
#7779=CARTESIAN_POINT('Ctrl Pts',(0.0129758042228726,1.19994565546462,-1.54874501349991));
#7780=CARTESIAN_POINT('Ctrl Pts',(0.0252945565319671,1.19974919586288,-1.54364210404195));
#7781=CARTESIAN_POINT('Ctrl Pts',(0.0309164568000038,1.19960989221221,-1.53979422131865));
#7782=CARTESIAN_POINT('Ctrl Pts',(0.0397942217705328,1.1993482149535,-1.53091645634812));
#7783=CARTESIAN_POINT('Ctrl Pts',(0.0436421041657012,1.19920885850753,-1.52529455629072));
#7784=CARTESIAN_POINT('Ctrl Pts',(0.048745013309908,1.19901227819454,-1.51297580462407));
#7785=CARTESIAN_POINT('Ctrl Pts',(0.05,1.19895788082818,-1.50627889147831));
#7786=CARTESIAN_POINT('Ctrl Pts',(0.05,1.19895788082818,-1.49372110852169));
#7787=CARTESIAN_POINT('Ctrl Pts',(0.0487450133099081,1.19901227819454,-1.48702419537594));
#7788=CARTESIAN_POINT('Ctrl Pts',(0.0436421041657014,1.19920885850753,-1.47470544370928));
#7789=CARTESIAN_POINT('Ctrl Pts',(0.0397942217705328,1.1993482149535,-1.46908354365188));
#7790=CARTESIAN_POINT('Ctrl Pts',(0.0309164568000038,1.19960989221221,-1.46020577868135));
#7791=CARTESIAN_POINT('Ctrl Pts',(0.0252945565319674,1.19974919586288,-1.45635789595805));
#7792=CARTESIAN_POINT('Ctrl Pts',(0.012975804222873,1.19994565546462,-1.45125498650009));
#7793=CARTESIAN_POINT('Ctrl Pts',(0.00627889083911038,1.2,-1.45));
#7794=CARTESIAN_POINT('Ctrl Pts',(-0.00627889083911039,1.2,-1.45));
#7795=CARTESIAN_POINT('Ctrl Pts',(-0.012975804222873,1.19994565546462,-1.45125498650009));
#7796=CARTESIAN_POINT('Ctrl Pts',(-0.0252945565319674,1.19974919586288,
-1.45635789595805));
#7797=CARTESIAN_POINT('Ctrl Pts',(-0.0309164568000038,1.19960989221221,
-1.46020577868135));
#7798=CARTESIAN_POINT('Ctrl Pts',(-0.0397942217705328,1.1993482149535,-1.46908354365188));
#7799=CARTESIAN_POINT('Ctrl Pts',(-0.0436421041657014,1.19920885850753,
-1.47470544370928));
#7800=CARTESIAN_POINT('Ctrl Pts',(-0.0487450133099081,1.19901227819454,
-1.48702419537594));
#7801=CARTESIAN_POINT('Ctrl Pts',(-0.05,1.19895788082818,-1.49372110852169));
#7802=CARTESIAN_POINT('Ctrl Pts',(-0.05,1.19895788082818,-1.5));
#7803=CARTESIAN_POINT('Origin',(0.,-1.3,-0.5));
#7804=CARTESIAN_POINT('',(-0.05,-1.19895788082818,-0.5));
#7805=CARTESIAN_POINT('Ctrl Pts',(-0.05,-1.19895788082818,-0.5));
#7806=CARTESIAN_POINT('Ctrl Pts',(-0.05,-1.19895788082818,-0.493721108521693));
#7807=CARTESIAN_POINT('Ctrl Pts',(-0.0487450133099082,-1.19901227819454,
-0.487024195375935));
#7808=CARTESIAN_POINT('Ctrl Pts',(-0.0436421041657013,-1.19920885850753,
-0.47470544370928));
#7809=CARTESIAN_POINT('Ctrl Pts',(-0.0397942217705328,-1.1993482149535,
-0.469083543651878));
#7810=CARTESIAN_POINT('Ctrl Pts',(-0.0309164568000038,-1.19960989221221,
-0.460205778681349));
#7811=CARTESIAN_POINT('Ctrl Pts',(-0.0252945565319674,-1.19974919586288,
-0.456357895958046));
#7812=CARTESIAN_POINT('Ctrl Pts',(-0.012975804222873,-1.19994565546462,
-0.451254986500089));
#7813=CARTESIAN_POINT('Ctrl Pts',(-0.00627889083911039,-1.2,-0.45));
#7814=CARTESIAN_POINT('Ctrl Pts',(0.00627889083911038,-1.2,-0.45));
#7815=CARTESIAN_POINT('Ctrl Pts',(0.012975804222873,-1.19994565546462,-0.451254986500089));
#7816=CARTESIAN_POINT('Ctrl Pts',(0.0252945565319674,-1.19974919586288,
-0.456357895958046));
#7817=CARTESIAN_POINT('Ctrl Pts',(0.0309164568000038,-1.19960989221221,
-0.460205778681349));
#7818=CARTESIAN_POINT('Ctrl Pts',(0.0397942217705328,-1.1993482149535,-0.469083543651878));
#7819=CARTESIAN_POINT('Ctrl Pts',(0.0436421041657013,-1.19920885850753,
-0.47470544370928));
#7820=CARTESIAN_POINT('Ctrl Pts',(0.0487450133099082,-1.19901227819454,
-0.487024195375935));
#7821=CARTESIAN_POINT('Ctrl Pts',(0.05,-1.19895788082818,-0.493721108521693));
#7822=CARTESIAN_POINT('Ctrl Pts',(0.05,-1.19895788082818,-0.506278891478307));
#7823=CARTESIAN_POINT('Ctrl Pts',(0.0487450133099082,-1.19901227819454,
-0.512975804624065));
#7824=CARTESIAN_POINT('Ctrl Pts',(0.0436421041657015,-1.19920885850753,
-0.52529455629072));
#7825=CARTESIAN_POINT('Ctrl Pts',(0.0397942217705327,-1.1993482149535,-0.530916456348121));
#7826=CARTESIAN_POINT('Ctrl Pts',(0.0309164568000038,-1.19960989221221,
-0.539794221318651));
#7827=CARTESIAN_POINT('Ctrl Pts',(0.0252945565319676,-1.19974919586288,
-0.543642104041954));
#7828=CARTESIAN_POINT('Ctrl Pts',(0.0129758042228732,-1.19994565546462,
-0.548745013499911));
#7829=CARTESIAN_POINT('Ctrl Pts',(0.00627889083911044,-1.2,-0.55));
#7830=CARTESIAN_POINT('Ctrl Pts',(-0.00627889083911041,-1.2,-0.55));
#7831=CARTESIAN_POINT('Ctrl Pts',(-0.0129758042228731,-1.19994565546462,
-0.548745013499911));
#7832=CARTESIAN_POINT('Ctrl Pts',(-0.0252945565319676,-1.19974919586288,
-0.543642104041954));
#7833=CARTESIAN_POINT('Ctrl Pts',(-0.0309164568000038,-1.19960989221221,
-0.539794221318651));
#7834=CARTESIAN_POINT('Ctrl Pts',(-0.0397942217705327,-1.1993482149535,
-0.530916456348121));
#7835=CARTESIAN_POINT('Ctrl Pts',(-0.0436421041657015,-1.19920885850753,
-0.52529455629072));
#7836=CARTESIAN_POINT('Ctrl Pts',(-0.0487450133099082,-1.19901227819454,
-0.512975804624065));
#7837=CARTESIAN_POINT('Ctrl Pts',(-0.05,-1.19895788082818,-0.506278891478307));
#7838=CARTESIAN_POINT('Ctrl Pts',(-0.05,-1.19895788082818,-0.5));
#7839=CARTESIAN_POINT('',(-0.05,-0.396862696659689,-0.5));
#7840=CARTESIAN_POINT('',(-0.05,-1.3,-0.5));
#7841=CARTESIAN_POINT('Ctrl Pts',(-0.05,-0.396862696659689,-0.5));
#7842=CARTESIAN_POINT('Ctrl Pts',(-0.05,-0.396862696659689,-0.506285200964255));
#7843=CARTESIAN_POINT('Ctrl Pts',(-0.0487425534891115,-0.397027412247524,
-0.512984801229014));
#7844=CARTESIAN_POINT('Ctrl Pts',(-0.0436378373878618,-0.397620851691571,
-0.525301794093861));
#7845=CARTESIAN_POINT('Ctrl Pts',(-0.0397909243921696,-0.398040841710914,
-0.530919753726485));
#7846=CARTESIAN_POINT('Ctrl Pts',(-0.0309197907817458,-0.398828027526425,
-0.539790887336909));
#7847=CARTESIAN_POINT('Ctrl Pts',(-0.0253018150396576,-0.399246581249293,
-0.543637829363298));
#7848=CARTESIAN_POINT('Ctrl Pts',(-0.0129847676279313,-0.399836729543542,
-0.548742566758595));
#7849=CARTESIAN_POINT('Ctrl Pts',(-0.00628514845714647,-0.4,-0.55));
#7850=CARTESIAN_POINT('Ctrl Pts',(0.00628514845714648,-0.4,-0.55));
#7851=CARTESIAN_POINT('Ctrl Pts',(0.0129847676279313,-0.399836729543542,
-0.548742566758595));
#7852=CARTESIAN_POINT('Ctrl Pts',(0.0253018150396576,-0.399246581249293,
-0.543637829363298));
#7853=CARTESIAN_POINT('Ctrl Pts',(0.0309197907817458,-0.398828027526425,
-0.539790887336909));
#7854=CARTESIAN_POINT('Ctrl Pts',(0.0397909243921696,-0.398040841710914,
-0.530919753726485));
#7855=CARTESIAN_POINT('Ctrl Pts',(0.0436378373878618,-0.397620851691571,
-0.525301794093861));
#7856=CARTESIAN_POINT('Ctrl Pts',(0.0487425534891115,-0.397027412247524,
-0.512984801229014));
#7857=CARTESIAN_POINT('Ctrl Pts',(0.05,-0.396862696659689,-0.506285200964255));
#7858=CARTESIAN_POINT('Ctrl Pts',(0.05,-0.396862696659689,-0.493714799035745));
#7859=CARTESIAN_POINT('Ctrl Pts',(0.0487425534891115,-0.397027412247524,
-0.487015198770986));
#7860=CARTESIAN_POINT('Ctrl Pts',(0.0436378373878618,-0.397620851691571,
-0.474698205906139));
#7861=CARTESIAN_POINT('Ctrl Pts',(0.0397909243921696,-0.398040841710914,
-0.469080246273515));
#7862=CARTESIAN_POINT('Ctrl Pts',(0.0309197907817458,-0.398828027526425,
-0.460209112663091));
#7863=CARTESIAN_POINT('Ctrl Pts',(0.0253018150396576,-0.399246581249293,
-0.456362170636702));
#7864=CARTESIAN_POINT('Ctrl Pts',(0.0129847676279313,-0.399836729543542,
-0.451257433241405));
#7865=CARTESIAN_POINT('Ctrl Pts',(0.00628514845714648,-0.4,-0.45));
#7866=CARTESIAN_POINT('Ctrl Pts',(-0.00628514845714647,-0.4,-0.45));
#7867=CARTESIAN_POINT('Ctrl Pts',(-0.0129847676279313,-0.399836729543542,
-0.451257433241405));
#7868=CARTESIAN_POINT('Ctrl Pts',(-0.0253018150396577,-0.399246581249293,
-0.456362170636702));
#7869=CARTESIAN_POINT('Ctrl Pts',(-0.0309197907817458,-0.398828027526425,
-0.460209112663091));
#7870=CARTESIAN_POINT('Ctrl Pts',(-0.0397909243921696,-0.398040841710914,
-0.469080246273515));
#7871=CARTESIAN_POINT('Ctrl Pts',(-0.0436378373878618,-0.397620851691571,
-0.474698205906139));
#7872=CARTESIAN_POINT('Ctrl Pts',(-0.0487425534891115,-0.397027412247524,
-0.487015198770986));
#7873=CARTESIAN_POINT('Ctrl Pts',(-0.05,-0.396862696659689,-0.493714799035745));
#7874=CARTESIAN_POINT('Ctrl Pts',(-0.05,-0.396862696659689,-0.5));
#7875=CARTESIAN_POINT('Origin',(0.,-1.3,-0.5));
#7876=CARTESIAN_POINT('',(-0.05,0.396862696659689,-0.5));
#7877=CARTESIAN_POINT('Ctrl Pts',(-0.05,0.396862696659689,-0.5));
#7878=CARTESIAN_POINT('Ctrl Pts',(-0.05,0.396862696659689,-0.493714799035745));
#7879=CARTESIAN_POINT('Ctrl Pts',(-0.0487425534891115,0.397027412247524,
-0.487015198770986));
#7880=CARTESIAN_POINT('Ctrl Pts',(-0.0436378373878618,0.397620851691571,
-0.474698205906139));
#7881=CARTESIAN_POINT('Ctrl Pts',(-0.0397909243921696,0.398040841710914,
-0.469080246273515));
#7882=CARTESIAN_POINT('Ctrl Pts',(-0.0309197907817458,0.398828027526425,
-0.460209112663091));
#7883=CARTESIAN_POINT('Ctrl Pts',(-0.0253018150396576,0.399246581249293,
-0.456362170636702));
#7884=CARTESIAN_POINT('Ctrl Pts',(-0.0129847676279312,0.399836729543542,
-0.451257433241405));
#7885=CARTESIAN_POINT('Ctrl Pts',(-0.00628514845714647,0.4,-0.45));
#7886=CARTESIAN_POINT('Ctrl Pts',(0.00628514845714648,0.4,-0.45));
#7887=CARTESIAN_POINT('Ctrl Pts',(0.0129847676279313,0.399836729543542,
-0.451257433241405));
#7888=CARTESIAN_POINT('Ctrl Pts',(0.0253018150396576,0.399246581249293,
-0.456362170636702));
#7889=CARTESIAN_POINT('Ctrl Pts',(0.0309197907817458,0.398828027526425,
-0.460209112663091));
#7890=CARTESIAN_POINT('Ctrl Pts',(0.0397909243921696,0.398040841710914,
-0.469080246273515));
#7891=CARTESIAN_POINT('Ctrl Pts',(0.0436378373878619,0.397620851691571,
-0.474698205906139));
#7892=CARTESIAN_POINT('Ctrl Pts',(0.0487425534891115,0.397027412247524,
-0.487015198770986));
#7893=CARTESIAN_POINT('Ctrl Pts',(0.05,0.396862696659689,-0.493714799035745));
#7894=CARTESIAN_POINT('Ctrl Pts',(0.05,0.396862696659689,-0.506285200964255));
#7895=CARTESIAN_POINT('Ctrl Pts',(0.0487425534891115,0.397027412247524,
-0.512984801229014));
#7896=CARTESIAN_POINT('Ctrl Pts',(0.0436378373878618,0.397620851691571,
-0.525301794093861));
#7897=CARTESIAN_POINT('Ctrl Pts',(0.0397909243921696,0.398040841710914,
-0.530919753726485));
#7898=CARTESIAN_POINT('Ctrl Pts',(0.0309197907817458,0.398828027526425,
-0.539790887336909));
#7899=CARTESIAN_POINT('Ctrl Pts',(0.0253018150396576,0.399246581249293,
-0.543637829363298));
#7900=CARTESIAN_POINT('Ctrl Pts',(0.0129847676279313,0.399836729543542,
-0.548742566758595));
#7901=CARTESIAN_POINT('Ctrl Pts',(0.00628514845714648,0.4,-0.55));
#7902=CARTESIAN_POINT('Ctrl Pts',(-0.00628514845714647,0.4,-0.55));
#7903=CARTESIAN_POINT('Ctrl Pts',(-0.0129847676279313,0.399836729543542,
-0.548742566758595));
#7904=CARTESIAN_POINT('Ctrl Pts',(-0.0253018150396576,0.399246581249293,
-0.543637829363298));
#7905=CARTESIAN_POINT('Ctrl Pts',(-0.0309197907817458,0.398828027526425,
-0.539790887336909));
#7906=CARTESIAN_POINT('Ctrl Pts',(-0.0397909243921696,0.398040841710914,
-0.530919753726485));
#7907=CARTESIAN_POINT('Ctrl Pts',(-0.0436378373878618,0.397620851691571,
-0.525301794093861));
#7908=CARTESIAN_POINT('Ctrl Pts',(-0.0487425534891115,0.397027412247524,
-0.512984801229014));
#7909=CARTESIAN_POINT('Ctrl Pts',(-0.05,0.396862696659689,-0.506285200964255));
#7910=CARTESIAN_POINT('Ctrl Pts',(-0.05,0.396862696659689,-0.5));
#7911=CARTESIAN_POINT('',(-0.05,1.19895788082818,-0.5));
#7912=CARTESIAN_POINT('',(-0.05,-1.3,-0.5));
#7913=CARTESIAN_POINT('Ctrl Pts',(-0.05,1.19895788082818,-0.5));
#7914=CARTESIAN_POINT('Ctrl Pts',(-0.05,1.19895788082818,-0.506278891478307));
#7915=CARTESIAN_POINT('Ctrl Pts',(-0.0487450133099082,1.19901227819454,
-0.512975804624065));
#7916=CARTESIAN_POINT('Ctrl Pts',(-0.0436421041657015,1.19920885850753,
-0.52529455629072));
#7917=CARTESIAN_POINT('Ctrl Pts',(-0.0397942217705327,1.1993482149535,-0.530916456348121));
#7918=CARTESIAN_POINT('Ctrl Pts',(-0.0309164568000038,1.19960989221221,
-0.539794221318651));
#7919=CARTESIAN_POINT('Ctrl Pts',(-0.0252945565319676,1.19974919586288,
-0.543642104041954));
#7920=CARTESIAN_POINT('Ctrl Pts',(-0.0129758042228731,1.19994565546462,
-0.548745013499911));
#7921=CARTESIAN_POINT('Ctrl Pts',(-0.0062788908391104,1.2,-0.55));
#7922=CARTESIAN_POINT('Ctrl Pts',(0.00627889083911043,1.2,-0.55));
#7923=CARTESIAN_POINT('Ctrl Pts',(0.0129758042228731,1.19994565546462,-0.548745013499911));
#7924=CARTESIAN_POINT('Ctrl Pts',(0.0252945565319676,1.19974919586288,-0.543642104041954));
#7925=CARTESIAN_POINT('Ctrl Pts',(0.0309164568000038,1.19960989221221,-0.539794221318651));
#7926=CARTESIAN_POINT('Ctrl Pts',(0.0397942217705327,1.1993482149535,-0.530916456348121));
#7927=CARTESIAN_POINT('Ctrl Pts',(0.0436421041657015,1.19920885850753,-0.52529455629072));
#7928=CARTESIAN_POINT('Ctrl Pts',(0.0487450133099082,1.19901227819454,-0.512975804624065));
#7929=CARTESIAN_POINT('Ctrl Pts',(0.05,1.19895788082818,-0.506278891478307));
#7930=CARTESIAN_POINT('Ctrl Pts',(0.05,1.19895788082818,-0.493721108521693));
#7931=CARTESIAN_POINT('Ctrl Pts',(0.0487450133099082,1.19901227819454,-0.487024195375935));
#7932=CARTESIAN_POINT('Ctrl Pts',(0.0436421041657013,1.19920885850753,-0.47470544370928));
#7933=CARTESIAN_POINT('Ctrl Pts',(0.0397942217705328,1.1993482149535,-0.469083543651878));
#7934=CARTESIAN_POINT('Ctrl Pts',(0.0309164568000038,1.19960989221221,-0.460205778681349));
#7935=CARTESIAN_POINT('Ctrl Pts',(0.0252945565319674,1.19974919586288,-0.456357895958046));
#7936=CARTESIAN_POINT('Ctrl Pts',(0.012975804222873,1.19994565546462,-0.451254986500089));
#7937=CARTESIAN_POINT('Ctrl Pts',(0.00627889083911038,1.2,-0.45));
#7938=CARTESIAN_POINT('Ctrl Pts',(-0.00627889083911039,1.2,-0.45));
#7939=CARTESIAN_POINT('Ctrl Pts',(-0.012975804222873,1.19994565546462,-0.451254986500089));
#7940=CARTESIAN_POINT('Ctrl Pts',(-0.0252945565319674,1.19974919586288,
-0.456357895958046));
#7941=CARTESIAN_POINT('Ctrl Pts',(-0.0309164568000038,1.19960989221221,
-0.460205778681349));
#7942=CARTESIAN_POINT('Ctrl Pts',(-0.0397942217705328,1.1993482149535,-0.469083543651878));
#7943=CARTESIAN_POINT('Ctrl Pts',(-0.0436421041657013,1.19920885850753,
-0.47470544370928));
#7944=CARTESIAN_POINT('Ctrl Pts',(-0.0487450133099082,1.19901227819454,
-0.487024195375935));
#7945=CARTESIAN_POINT('Ctrl Pts',(-0.05,1.19895788082818,-0.493721108521693));
#7946=CARTESIAN_POINT('Ctrl Pts',(-0.05,1.19895788082818,-0.5));
#7947=CARTESIAN_POINT('Origin',(-1.3,0.,-2.5));
#7948=CARTESIAN_POINT('',(-1.19895788082818,0.0499999999999998,-2.5));
#7949=CARTESIAN_POINT('',(-1.2,-6.12323399573674E-18,-2.45));
#7950=CARTESIAN_POINT('Ctrl Pts',(-1.19895788082818,0.0499999999999998,
-2.5));
#7951=CARTESIAN_POINT('Ctrl Pts',(-1.19895788082818,0.0499999999999998,
-2.49372110852169));
#7952=CARTESIAN_POINT('Ctrl Pts',(-1.19901227819454,0.0487450133099079,
-2.48702419537593));
#7953=CARTESIAN_POINT('Ctrl Pts',(-1.19920885850753,0.0436421041657012,
-2.47470544370928));
#7954=CARTESIAN_POINT('Ctrl Pts',(-1.1993482149535,0.0397942217705327,-2.46908354365188));
#7955=CARTESIAN_POINT('Ctrl Pts',(-1.19960989221221,0.0309164568000037,
-2.46020577868135));
#7956=CARTESIAN_POINT('Ctrl Pts',(-1.19974919586288,0.0252945565319673,
-2.45635789595805));
#7957=CARTESIAN_POINT('Ctrl Pts',(-1.19994565546462,0.0129758042228729,
-2.45125498650009));
#7958=CARTESIAN_POINT('Ctrl Pts',(-1.2,0.00627889083911036,-2.45));
#7959=CARTESIAN_POINT('Ctrl Pts',(-1.2,6.07153216591882E-18,-2.45));
#7960=CARTESIAN_POINT('',(-1.2,-7.88998188112687E-17,-2.55));
#7961=CARTESIAN_POINT('Ctrl Pts',(-1.2,-1.0842021724855E-17,-2.55));
#7962=CARTESIAN_POINT('Ctrl Pts',(-1.2,0.00627889083911035,-2.55));
#7963=CARTESIAN_POINT('Ctrl Pts',(-1.19994565546462,0.0129758042228729,
-2.54874501349991));
#7964=CARTESIAN_POINT('Ctrl Pts',(-1.19974919586288,0.0252945565319673,
-2.54364210404195));
#7965=CARTESIAN_POINT('Ctrl Pts',(-1.19960989221221,0.0309164568000037,
-2.53979422131865));
#7966=CARTESIAN_POINT('Ctrl Pts',(-1.1993482149535,0.0397942217705327,-2.53091645634812));
#7967=CARTESIAN_POINT('Ctrl Pts',(-1.19920885850753,0.0436421041657012,
-2.52529455629072));
#7968=CARTESIAN_POINT('Ctrl Pts',(-1.19901227819454,0.0487450133099079,
-2.51297580462407));
#7969=CARTESIAN_POINT('Ctrl Pts',(-1.19895788082818,0.0499999999999998,
-2.50627889147831));
#7970=CARTESIAN_POINT('Ctrl Pts',(-1.19895788082818,0.0499999999999998,
-2.5));
#7971=CARTESIAN_POINT('Ctrl Pts',(-1.2,6.07153216591882E-18,-2.45));
#7972=CARTESIAN_POINT('Ctrl Pts',(-1.2,-0.00627889083911035,-2.45));
#7973=CARTESIAN_POINT('Ctrl Pts',(-1.19994565546462,-0.0129758042228729,
-2.45125498650009));
#7974=CARTESIAN_POINT('Ctrl Pts',(-1.19974919586288,-0.0252945565319673,
-2.45635789595805));
#7975=CARTESIAN_POINT('Ctrl Pts',(-1.19960989221221,-0.0309164568000037,
-2.46020577868135));
#7976=CARTESIAN_POINT('Ctrl Pts',(-1.1993482149535,-0.0397942217705327,
-2.46908354365188));
#7977=CARTESIAN_POINT('Ctrl Pts',(-1.19920885850753,-0.0436421041657012,
-2.47470544370928));
#7978=CARTESIAN_POINT('Ctrl Pts',(-1.19901227819454,-0.0487450133099079,
-2.48702419537593));
#7979=CARTESIAN_POINT('Ctrl Pts',(-1.19895788082818,-0.0499999999999998,
-2.49372110852169));
#7980=CARTESIAN_POINT('Ctrl Pts',(-1.19895788082818,-0.0499999999999998,
-2.50627889147831));
#7981=CARTESIAN_POINT('Ctrl Pts',(-1.19901227819454,-0.0487450133099079,
-2.51297580462407));
#7982=CARTESIAN_POINT('Ctrl Pts',(-1.19920885850753,-0.0436421041657012,
-2.52529455629072));
#7983=CARTESIAN_POINT('Ctrl Pts',(-1.1993482149535,-0.0397942217705327,
-2.53091645634812));
#7984=CARTESIAN_POINT('Ctrl Pts',(-1.19960989221221,-0.0309164568000037,
-2.53979422131865));
#7985=CARTESIAN_POINT('Ctrl Pts',(-1.19974919586288,-0.0252945565319673,
-2.54364210404195));
#7986=CARTESIAN_POINT('Ctrl Pts',(-1.19994565546462,-0.0129758042228729,
-2.54874501349991));
#7987=CARTESIAN_POINT('Ctrl Pts',(-1.2,-0.00627889083911037,-2.55));
#7988=CARTESIAN_POINT('Ctrl Pts',(-1.2,-1.0842021724855E-17,-2.55));
#7989=CARTESIAN_POINT('',(-0.4,-6.53106394982199E-18,-2.45));
#7990=CARTESIAN_POINT('',(-1.3,-6.12323399573674E-18,-2.45));
#7991=CARTESIAN_POINT('',(-0.4,-2.44929359829471E-17,-2.55));
#7992=CARTESIAN_POINT('Ctrl Pts',(-0.4,0.,-2.55));
#7993=CARTESIAN_POINT('Ctrl Pts',(-0.4,-0.00628514845714645,-2.55));
#7994=CARTESIAN_POINT('Ctrl Pts',(-0.399836729543542,-0.0129847676279312,
-2.5487425667586));
#7995=CARTESIAN_POINT('Ctrl Pts',(-0.399246581249293,-0.0253018150396575,
-2.5436378293633));
#7996=CARTESIAN_POINT('Ctrl Pts',(-0.398828027526425,-0.0309197907817456,
-2.53979088733691));
#7997=CARTESIAN_POINT('Ctrl Pts',(-0.398040841710914,-0.0397909243921695,
-2.53091975372649));
#7998=CARTESIAN_POINT('Ctrl Pts',(-0.397620851691571,-0.0436378373878614,
-2.52530179409386));
#7999=CARTESIAN_POINT('Ctrl Pts',(-0.397027412247524,-0.0487425534891113,
-2.51298480122901));
#8000=CARTESIAN_POINT('Ctrl Pts',(-0.396862696659689,-0.0499999999999998,
-2.50628520096426));
#8001=CARTESIAN_POINT('Ctrl Pts',(-0.396862696659689,-0.0499999999999998,
-2.49371479903574));
#8002=CARTESIAN_POINT('Ctrl Pts',(-0.397027412247524,-0.0487425534891114,
-2.48701519877099));
#8003=CARTESIAN_POINT('Ctrl Pts',(-0.397620851691571,-0.0436378373878616,
-2.47469820590614));
#8004=CARTESIAN_POINT('Ctrl Pts',(-0.398040841710914,-0.0397909243921695,
-2.46908024627351));
#8005=CARTESIAN_POINT('Ctrl Pts',(-0.398828027526425,-0.0309197907817457,
-2.46020911266309));
#8006=CARTESIAN_POINT('Ctrl Pts',(-0.399246581249293,-0.0253018150396575,
-2.4563621706367));
#8007=CARTESIAN_POINT('Ctrl Pts',(-0.399836729543542,-0.0129847676279312,
-2.4512574332414));
#8008=CARTESIAN_POINT('Ctrl Pts',(-0.4,-0.00628514845714645,-2.45));
#8009=CARTESIAN_POINT('Ctrl Pts',(-0.4,-6.93889390390723E-18,-2.45));
#8010=CARTESIAN_POINT('',(-0.396862696659689,0.0499999999999998,-2.5));
#8011=CARTESIAN_POINT('Ctrl Pts',(-0.396862696659689,0.0499999999999998,
-2.5));
#8012=CARTESIAN_POINT('Ctrl Pts',(-0.396862696659689,0.0499999999999998,
-2.50628520096426));
#8013=CARTESIAN_POINT('Ctrl Pts',(-0.397027412247524,0.0487425534891114,
-2.51298480122901));
#8014=CARTESIAN_POINT('Ctrl Pts',(-0.397620851691571,0.0436378373878616,
-2.52530179409386));
#8015=CARTESIAN_POINT('Ctrl Pts',(-0.398040841710914,0.0397909243921695,
-2.53091975372649));
#8016=CARTESIAN_POINT('Ctrl Pts',(-0.398828027526425,0.0309197907817456,
-2.53979088733691));
#8017=CARTESIAN_POINT('Ctrl Pts',(-0.399246581249293,0.0253018150396575,
-2.5436378293633));
#8018=CARTESIAN_POINT('Ctrl Pts',(-0.399836729543542,0.0129847676279312,
-2.5487425667586));
#8019=CARTESIAN_POINT('Ctrl Pts',(-0.4,0.00628514845714645,-2.55));
#8020=CARTESIAN_POINT('Ctrl Pts',(-0.4,0.,-2.55));
#8021=CARTESIAN_POINT('Ctrl Pts',(-0.4,-6.93889390390723E-18,-2.45));
#8022=CARTESIAN_POINT('Ctrl Pts',(-0.4,0.00628514845714644,-2.45));
#8023=CARTESIAN_POINT('Ctrl Pts',(-0.399836729543542,0.0129847676279312,
-2.4512574332414));
#8024=CARTESIAN_POINT('Ctrl Pts',(-0.399246581249293,0.0253018150396575,
-2.4563621706367));
#8025=CARTESIAN_POINT('Ctrl Pts',(-0.398828027526425,0.0309197907817456,
-2.46020911266309));
#8026=CARTESIAN_POINT('Ctrl Pts',(-0.398040841710914,0.0397909243921695,
-2.46908024627351));
#8027=CARTESIAN_POINT('Ctrl Pts',(-0.397620851691571,0.0436378373878614,
-2.47469820590614));
#8028=CARTESIAN_POINT('Ctrl Pts',(-0.397027412247524,0.0487425534891113,
-2.48701519877099));
#8029=CARTESIAN_POINT('Ctrl Pts',(-0.396862696659689,0.0499999999999998,
-2.49371479903574));
#8030=CARTESIAN_POINT('Ctrl Pts',(-0.396862696659689,0.0499999999999998,
-2.5));
#8031=CARTESIAN_POINT('Origin',(-1.3,0.,-2.5));
#8032=CARTESIAN_POINT('',(0.396862696659689,0.0499999999999998,-2.5));
#8033=CARTESIAN_POINT('',(0.4,-6.74790438431909E-18,-2.45));
#8034=CARTESIAN_POINT('Ctrl Pts',(0.396862696659689,0.0499999999999998,
-2.5));
#8035=CARTESIAN_POINT('Ctrl Pts',(0.396862696659689,0.0499999999999998,
-2.49371479903574));
#8036=CARTESIAN_POINT('Ctrl Pts',(0.397027412247524,0.0487425534891114,
-2.48701519877099));
#8037=CARTESIAN_POINT('Ctrl Pts',(0.397620851691571,0.0436378373878616,
-2.47469820590614));
#8038=CARTESIAN_POINT('Ctrl Pts',(0.398040841710914,0.0397909243921695,
-2.46908024627351));
#8039=CARTESIAN_POINT('Ctrl Pts',(0.398828027526425,0.0309197907817456,
-2.46020911266309));
#8040=CARTESIAN_POINT('Ctrl Pts',(0.399246581249293,0.0253018150396575,
-2.4563621706367));
#8041=CARTESIAN_POINT('Ctrl Pts',(0.399836729543542,0.0129847676279312,
-2.4512574332414));
#8042=CARTESIAN_POINT('Ctrl Pts',(0.4,0.00628514845714644,-2.45));
#8043=CARTESIAN_POINT('Ctrl Pts',(0.4,-7.37257477290143E-18,-2.45));
#8044=CARTESIAN_POINT('Ctrl Pts',(0.4,-7.37257477290143E-18,-2.45));
#8045=CARTESIAN_POINT('Ctrl Pts',(0.4,-0.00628514845714645,-2.45));
#8046=CARTESIAN_POINT('Ctrl Pts',(0.399836729543542,-0.0129847676279312,
-2.4512574332414));
#8047=CARTESIAN_POINT('Ctrl Pts',(0.399246581249293,-0.0253018150396575,
-2.4563621706367));
#8048=CARTESIAN_POINT('Ctrl Pts',(0.398828027526425,-0.0309197907817457,
-2.46020911266309));
#8049=CARTESIAN_POINT('Ctrl Pts',(0.398040841710914,-0.0397909243921695,
-2.46908024627351));
#8050=CARTESIAN_POINT('Ctrl Pts',(0.397620851691571,-0.0436378373878616,
-2.47469820590614));
#8051=CARTESIAN_POINT('Ctrl Pts',(0.397027412247524,-0.0487425534891114,
-2.48701519877099));
#8052=CARTESIAN_POINT('Ctrl Pts',(0.396862696659689,-0.0499999999999998,
-2.49371479903574));
#8053=CARTESIAN_POINT('Ctrl Pts',(0.396862696659689,-0.0499999999999998,
-2.50628520096426));
#8054=CARTESIAN_POINT('Ctrl Pts',(0.397027412247524,-0.0487425534891113,
-2.51298480122901));
#8055=CARTESIAN_POINT('Ctrl Pts',(0.397620851691571,-0.0436378373878614,
-2.52530179409386));
#8056=CARTESIAN_POINT('Ctrl Pts',(0.398040841710914,-0.0397909243921695,
-2.53091975372649));
#8057=CARTESIAN_POINT('Ctrl Pts',(0.398828027526425,-0.0309197907817457,
-2.53979088733691));
#8058=CARTESIAN_POINT('Ctrl Pts',(0.399246581249293,-0.0253018150396572,
-2.5436378293633));
#8059=CARTESIAN_POINT('Ctrl Pts',(0.399836729543542,-0.0129847676279309,
-2.5487425667586));
#8060=CARTESIAN_POINT('Ctrl Pts',(0.4,-0.00628514845714645,-2.55));
#8061=CARTESIAN_POINT('Ctrl Pts',(0.4,0.00628514845714645,-2.55));
#8062=CARTESIAN_POINT('Ctrl Pts',(0.399836729543542,0.0129847676279312,
-2.5487425667586));
#8063=CARTESIAN_POINT('Ctrl Pts',(0.399246581249293,0.0253018150396575,
-2.5436378293633));
#8064=CARTESIAN_POINT('Ctrl Pts',(0.398828027526425,0.0309197907817456,
-2.53979088733691));
#8065=CARTESIAN_POINT('Ctrl Pts',(0.398040841710914,0.0397909243921695,
-2.53091975372649));
#8066=CARTESIAN_POINT('Ctrl Pts',(0.397620851691571,0.0436378373878616,
-2.52530179409386));
#8067=CARTESIAN_POINT('Ctrl Pts',(0.397027412247524,0.0487425534891114,
-2.51298480122901));
#8068=CARTESIAN_POINT('Ctrl Pts',(0.396862696659689,0.0499999999999998,
-2.50628520096426));
#8069=CARTESIAN_POINT('Ctrl Pts',(0.396862696659689,0.0499999999999998,
-2.5));
#8070=CARTESIAN_POINT('',(1.2,-6.12323399573674E-18,-2.45));
#8071=CARTESIAN_POINT('',(-1.3,-6.12323399573674E-18,-2.45));
#8072=CARTESIAN_POINT('',(1.19895788082818,0.0499999999999998,-2.5));
#8073=CARTESIAN_POINT('Ctrl Pts',(1.19895788082818,0.0499999999999998,-2.5));
#8074=CARTESIAN_POINT('Ctrl Pts',(1.19895788082818,0.0499999999999998,-2.50627889147831));
#8075=CARTESIAN_POINT('Ctrl Pts',(1.19901227819454,0.0487450133099079,-2.51297580462407));
#8076=CARTESIAN_POINT('Ctrl Pts',(1.19920885850753,0.0436421041657012,-2.52529455629072));
#8077=CARTESIAN_POINT('Ctrl Pts',(1.1993482149535,0.0397942217705327,-2.53091645634812));
#8078=CARTESIAN_POINT('Ctrl Pts',(1.19960989221221,0.0309164568000037,-2.53979422131865));
#8079=CARTESIAN_POINT('Ctrl Pts',(1.19974919586288,0.0252945565319673,-2.54364210404195));
#8080=CARTESIAN_POINT('Ctrl Pts',(1.19994565546462,0.0129758042228729,-2.54874501349991));
#8081=CARTESIAN_POINT('Ctrl Pts',(1.2,0.00627889083911035,-2.55));
#8082=CARTESIAN_POINT('Ctrl Pts',(1.2,-0.00627889083911037,-2.55));
#8083=CARTESIAN_POINT('Ctrl Pts',(1.19994565546462,-0.0129758042228729,
-2.54874501349991));
#8084=CARTESIAN_POINT('Ctrl Pts',(1.19974919586288,-0.0252945565319673,
-2.54364210404195));
#8085=CARTESIAN_POINT('Ctrl Pts',(1.19960989221221,-0.0309164568000037,
-2.53979422131865));
#8086=CARTESIAN_POINT('Ctrl Pts',(1.1993482149535,-0.0397942217705327,-2.53091645634812));
#8087=CARTESIAN_POINT('Ctrl Pts',(1.19920885850753,-0.0436421041657012,
-2.52529455629072));
#8088=CARTESIAN_POINT('Ctrl Pts',(1.19901227819454,-0.0487450133099079,
-2.51297580462407));
#8089=CARTESIAN_POINT('Ctrl Pts',(1.19895788082818,-0.0499999999999998,
-2.50627889147831));
#8090=CARTESIAN_POINT('Ctrl Pts',(1.19895788082818,-0.0499999999999998,
-2.49372110852169));
#8091=CARTESIAN_POINT('Ctrl Pts',(1.19901227819454,-0.0487450133099081,
-2.48702419537594));
#8092=CARTESIAN_POINT('Ctrl Pts',(1.19920885850753,-0.0436421041657014,
-2.47470544370928));
#8093=CARTESIAN_POINT('Ctrl Pts',(1.1993482149535,-0.0397942217705327,-2.46908354365188));
#8094=CARTESIAN_POINT('Ctrl Pts',(1.19960989221221,-0.0309164568000037,
-2.46020577868135));
#8095=CARTESIAN_POINT('Ctrl Pts',(1.19974919586288,-0.0252945565319673,
-2.45635789595805));
#8096=CARTESIAN_POINT('Ctrl Pts',(1.19994565546462,-0.0129758042228729,
-2.45125498650009));
#8097=CARTESIAN_POINT('Ctrl Pts',(1.2,-0.00627889083911035,-2.45));
#8098=CARTESIAN_POINT('Ctrl Pts',(1.2,6.07153216591882E-18,-2.45));
#8099=CARTESIAN_POINT('Ctrl Pts',(1.2,6.07153216591882E-18,-2.45));
#8100=CARTESIAN_POINT('Ctrl Pts',(1.2,0.00627889083911036,-2.45));
#8101=CARTESIAN_POINT('Ctrl Pts',(1.19994565546462,0.0129758042228729,-2.45125498650009));
#8102=CARTESIAN_POINT('Ctrl Pts',(1.19974919586288,0.0252945565319673,-2.45635789595805));
#8103=CARTESIAN_POINT('Ctrl Pts',(1.19960989221221,0.0309164568000037,-2.46020577868135));
#8104=CARTESIAN_POINT('Ctrl Pts',(1.1993482149535,0.0397942217705327,-2.46908354365188));
#8105=CARTESIAN_POINT('Ctrl Pts',(1.19920885850753,0.0436421041657012,-2.47470544370928));
#8106=CARTESIAN_POINT('Ctrl Pts',(1.19901227819454,0.0487450133099079,-2.48702419537593));
#8107=CARTESIAN_POINT('Ctrl Pts',(1.19895788082818,0.0499999999999998,-2.49372110852169));
#8108=CARTESIAN_POINT('Ctrl Pts',(1.19895788082818,0.0499999999999998,-2.5));
#8109=CARTESIAN_POINT('Origin',(-1.3,0.,-1.5));
#8110=CARTESIAN_POINT('',(-1.19895788082818,0.05,-1.5));
#8111=CARTESIAN_POINT('',(-1.2,-6.12323399573677E-18,-1.45));
#8112=CARTESIAN_POINT('Ctrl Pts',(-1.19895788082818,0.05,-1.5));
#8113=CARTESIAN_POINT('Ctrl Pts',(-1.19895788082818,0.05,-1.49372110852169));
#8114=CARTESIAN_POINT('Ctrl Pts',(-1.19901227819454,0.0487450133099082,
-1.48702419537594));
#8115=CARTESIAN_POINT('Ctrl Pts',(-1.19920885850753,0.0436421041657014,
-1.47470544370928));
#8116=CARTESIAN_POINT('Ctrl Pts',(-1.1993482149535,0.0397942217705329,-1.46908354365188));
#8117=CARTESIAN_POINT('Ctrl Pts',(-1.19960989221221,0.0309164568000038,
-1.46020577868135));
#8118=CARTESIAN_POINT('Ctrl Pts',(-1.19974919586288,0.0252945565319674,
-1.45635789595805));
#8119=CARTESIAN_POINT('Ctrl Pts',(-1.19994565546462,0.012975804222873,-1.45125498650009));
#8120=CARTESIAN_POINT('Ctrl Pts',(-1.2,0.00627889083911039,-1.45));
#8121=CARTESIAN_POINT('Ctrl Pts',(-1.2,7.37257477290143E-18,-1.45));
#8122=CARTESIAN_POINT('',(-1.2,-7.84661379422745E-17,-1.55));
#8123=CARTESIAN_POINT('Ctrl Pts',(-1.2,-9.97465998686664E-18,-1.55));
#8124=CARTESIAN_POINT('Ctrl Pts',(-1.2,0.00627889083911038,-1.55));
#8125=CARTESIAN_POINT('Ctrl Pts',(-1.19994565546462,0.0129758042228729,
-1.54874501349991));
#8126=CARTESIAN_POINT('Ctrl Pts',(-1.19974919586288,0.0252945565319674,
-1.54364210404195));
#8127=CARTESIAN_POINT('Ctrl Pts',(-1.19960989221221,0.0309164568000038,
-1.53979422131865));
#8128=CARTESIAN_POINT('Ctrl Pts',(-1.1993482149535,0.0397942217705328,-1.53091645634812));
#8129=CARTESIAN_POINT('Ctrl Pts',(-1.19920885850753,0.0436421041657013,
-1.52529455629072));
#8130=CARTESIAN_POINT('Ctrl Pts',(-1.19901227819454,0.0487450133099081,
-1.51297580462407));
#8131=CARTESIAN_POINT('Ctrl Pts',(-1.19895788082818,0.05,-1.50627889147831));
#8132=CARTESIAN_POINT('Ctrl Pts',(-1.19895788082818,0.05,-1.5));
#8133=CARTESIAN_POINT('Ctrl Pts',(-1.2,7.37257477290143E-18,-1.45));
#8134=CARTESIAN_POINT('Ctrl Pts',(-1.2,-0.00627889083911038,-1.45));
#8135=CARTESIAN_POINT('Ctrl Pts',(-1.19994565546462,-0.0129758042228731,
-1.45125498650009));
#8136=CARTESIAN_POINT('Ctrl Pts',(-1.19974919586288,-0.0252945565319675,
-1.45635789595805));
#8137=CARTESIAN_POINT('Ctrl Pts',(-1.19960989221221,-0.0309164568000038,
-1.46020577868135));
#8138=CARTESIAN_POINT('Ctrl Pts',(-1.1993482149535,-0.0397942217705328,
-1.46908354365188));
#8139=CARTESIAN_POINT('Ctrl Pts',(-1.19920885850753,-0.0436421041657014,
-1.47470544370928));
#8140=CARTESIAN_POINT('Ctrl Pts',(-1.19901227819454,-0.0487450133099082,
-1.48702419537594));
#8141=CARTESIAN_POINT('Ctrl Pts',(-1.19895788082818,-0.05,-1.49372110852169));
#8142=CARTESIAN_POINT('Ctrl Pts',(-1.19895788082818,-0.05,-1.50627889147831));
#8143=CARTESIAN_POINT('Ctrl Pts',(-1.19901227819454,-0.0487450133099082,
-1.51297580462406));
#8144=CARTESIAN_POINT('Ctrl Pts',(-1.19920885850753,-0.0436421041657014,
-1.52529455629072));
#8145=CARTESIAN_POINT('Ctrl Pts',(-1.1993482149535,-0.0397942217705328,
-1.53091645634812));
#8146=CARTESIAN_POINT('Ctrl Pts',(-1.19960989221221,-0.0309164568000038,
-1.53979422131865));
#8147=CARTESIAN_POINT('Ctrl Pts',(-1.19974919586288,-0.0252945565319672,
-1.54364210404195));
#8148=CARTESIAN_POINT('Ctrl Pts',(-1.19994565546462,-0.0129758042228727,
-1.54874501349991));
#8149=CARTESIAN_POINT('Ctrl Pts',(-1.2,-0.0062788908391104,-1.55));
#8150=CARTESIAN_POINT('Ctrl Pts',(-1.2,-9.97465998686664E-18,-1.55));
#8151=CARTESIAN_POINT('',(-0.4,-6.0973830808278E-18,-1.45));
#8152=CARTESIAN_POINT('',(-1.3,-6.12323399573677E-18,-1.45));
#8153=CARTESIAN_POINT('',(-0.4,-2.427609554845E-17,-1.55));
#8154=CARTESIAN_POINT('Ctrl Pts',(-0.4,4.33680868994202E-19,-1.55));
#8155=CARTESIAN_POINT('Ctrl Pts',(-0.4,-0.00628514845714649,-1.55));
#8156=CARTESIAN_POINT('Ctrl Pts',(-0.399836729543542,-0.0129847676279311,
-1.5487425667586));
#8157=CARTESIAN_POINT('Ctrl Pts',(-0.399246581249293,-0.0253018150396574,
-1.5436378293633));
#8158=CARTESIAN_POINT('Ctrl Pts',(-0.398828027526425,-0.0309197907817458,
-1.53979088733691));
#8159=CARTESIAN_POINT('Ctrl Pts',(-0.398040841710914,-0.0397909243921696,
-1.53091975372649));
#8160=CARTESIAN_POINT('Ctrl Pts',(-0.397620851691571,-0.0436378373878618,
-1.52530179409386));
#8161=CARTESIAN_POINT('Ctrl Pts',(-0.397027412247524,-0.0487425534891115,
-1.51298480122901));
#8162=CARTESIAN_POINT('Ctrl Pts',(-0.396862696659689,-0.05,-1.50628520096426));
#8163=CARTESIAN_POINT('Ctrl Pts',(-0.396862696659689,-0.05,-1.49371479903575));
#8164=CARTESIAN_POINT('Ctrl Pts',(-0.397027412247524,-0.0487425534891117,
-1.48701519877099));
#8165=CARTESIAN_POINT('Ctrl Pts',(-0.397620851691571,-0.0436378373878621,
-1.47469820590614));
#8166=CARTESIAN_POINT('Ctrl Pts',(-0.398040841710914,-0.0397909243921697,
-1.46908024627352));
#8167=CARTESIAN_POINT('Ctrl Pts',(-0.398828027526425,-0.0309197907817458,
-1.46020911266309));
#8168=CARTESIAN_POINT('Ctrl Pts',(-0.399246581249293,-0.0253018150396577,
-1.4563621706367));
#8169=CARTESIAN_POINT('Ctrl Pts',(-0.399836729543542,-0.0129847676279314,
-1.4512574332414));
#8170=CARTESIAN_POINT('Ctrl Pts',(-0.4,-0.00628514845714648,-1.45));
#8171=CARTESIAN_POINT('Ctrl Pts',(-0.4,-6.07153216591882E-18,-1.45));
#8172=CARTESIAN_POINT('',(-0.396862696659689,0.05,-1.5));
#8173=CARTESIAN_POINT('Ctrl Pts',(-0.396862696659689,0.05,-1.5));
#8174=CARTESIAN_POINT('Ctrl Pts',(-0.396862696659689,0.05,-1.50628520096425));
#8175=CARTESIAN_POINT('Ctrl Pts',(-0.397027412247524,0.0487425534891116,
-1.51298480122901));
#8176=CARTESIAN_POINT('Ctrl Pts',(-0.397620851691571,0.0436378373878619,
-1.52530179409386));
#8177=CARTESIAN_POINT('Ctrl Pts',(-0.398040841710914,0.0397909243921696,
-1.53091975372649));
#8178=CARTESIAN_POINT('Ctrl Pts',(-0.398828027526425,0.0309197907817458,
-1.53979088733691));
#8179=CARTESIAN_POINT('Ctrl Pts',(-0.399246581249293,0.0253018150396575,
-1.5436378293633));
#8180=CARTESIAN_POINT('Ctrl Pts',(-0.399836729543542,0.0129847676279312,
-1.54874256675859));
#8181=CARTESIAN_POINT('Ctrl Pts',(-0.4,0.00628514845714648,-1.55));
#8182=CARTESIAN_POINT('Ctrl Pts',(-0.4,4.33680868994202E-19,-1.55));
#8183=CARTESIAN_POINT('Ctrl Pts',(-0.4,-6.07153216591882E-18,-1.45));
#8184=CARTESIAN_POINT('Ctrl Pts',(-0.4,0.00628514845714647,-1.45));
#8185=CARTESIAN_POINT('Ctrl Pts',(-0.399836729543542,0.0129847676279314,
-1.45125743324141));
#8186=CARTESIAN_POINT('Ctrl Pts',(-0.399246581249293,0.0253018150396577,
-1.4563621706367));
#8187=CARTESIAN_POINT('Ctrl Pts',(-0.398828027526425,0.0309197907817458,
-1.46020911266309));
#8188=CARTESIAN_POINT('Ctrl Pts',(-0.398040841710914,0.0397909243921697,
-1.46908024627351));
#8189=CARTESIAN_POINT('Ctrl Pts',(-0.397620851691571,0.0436378373878618,
-1.47469820590614));
#8190=CARTESIAN_POINT('Ctrl Pts',(-0.397027412247524,0.0487425534891115,
-1.48701519877099));
#8191=CARTESIAN_POINT('Ctrl Pts',(-0.396862696659689,0.05,-1.49371479903574));
#8192=CARTESIAN_POINT('Ctrl Pts',(-0.396862696659689,0.05,-1.5));
#8193=CARTESIAN_POINT('Origin',(-1.3,0.,-1.5));
#8194=CARTESIAN_POINT('',(0.396862696659689,0.05,-1.5));
#8195=CARTESIAN_POINT('',(0.4,-6.3142235153249E-18,-1.45));
#8196=CARTESIAN_POINT('Ctrl Pts',(0.396862696659689,0.05,-1.5));
#8197=CARTESIAN_POINT('Ctrl Pts',(0.396862696659689,0.05,-1.49371479903575));
#8198=CARTESIAN_POINT('Ctrl Pts',(0.397027412247524,0.0487425534891116,
-1.48701519877099));
#8199=CARTESIAN_POINT('Ctrl Pts',(0.397620851691571,0.0436378373878619,
-1.47469820590614));
#8200=CARTESIAN_POINT('Ctrl Pts',(0.398040841710914,0.0397909243921697,
-1.46908024627351));
#8201=CARTESIAN_POINT('Ctrl Pts',(0.398828027526425,0.0309197907817458,
-1.46020911266309));
#8202=CARTESIAN_POINT('Ctrl Pts',(0.399246581249293,0.0253018150396577,
-1.4563621706367));
#8203=CARTESIAN_POINT('Ctrl Pts',(0.399836729543542,0.0129847676279313,
-1.4512574332414));
#8204=CARTESIAN_POINT('Ctrl Pts',(0.4,0.00628514845714647,-1.45));
#8205=CARTESIAN_POINT('Ctrl Pts',(0.4,-6.50521303491303E-18,-1.45));
#8206=CARTESIAN_POINT('Ctrl Pts',(0.4,-6.50521303491303E-18,-1.45));
#8207=CARTESIAN_POINT('Ctrl Pts',(0.4,-0.00628514845714648,-1.45));
#8208=CARTESIAN_POINT('Ctrl Pts',(0.399836729543542,-0.0129847676279314,
-1.4512574332414));
#8209=CARTESIAN_POINT('Ctrl Pts',(0.399246581249293,-0.0253018150396577,
-1.4563621706367));
#8210=CARTESIAN_POINT('Ctrl Pts',(0.398828027526425,-0.0309197907817458,
-1.46020911266309));
#8211=CARTESIAN_POINT('Ctrl Pts',(0.398040841710914,-0.0397909243921697,
-1.46908024627351));
#8212=CARTESIAN_POINT('Ctrl Pts',(0.397620851691571,-0.0436378373878622,
-1.47469820590614));
#8213=CARTESIAN_POINT('Ctrl Pts',(0.397027412247524,-0.0487425534891117,
-1.48701519877099));
#8214=CARTESIAN_POINT('Ctrl Pts',(0.396862696659689,-0.05,-1.49371479903575));
#8215=CARTESIAN_POINT('Ctrl Pts',(0.396862696659689,-0.05,-1.50628520096425));
#8216=CARTESIAN_POINT('Ctrl Pts',(0.397027412247524,-0.0487425534891116,
-1.51298480122901));
#8217=CARTESIAN_POINT('Ctrl Pts',(0.397620851691571,-0.0436378373878619,
-1.52530179409386));
#8218=CARTESIAN_POINT('Ctrl Pts',(0.398040841710914,-0.0397909243921696,
-1.53091975372649));
#8219=CARTESIAN_POINT('Ctrl Pts',(0.398828027526425,-0.0309197907817458,
-1.53979088733691));
#8220=CARTESIAN_POINT('Ctrl Pts',(0.399246581249293,-0.0253018150396575,
-1.5436378293633));
#8221=CARTESIAN_POINT('Ctrl Pts',(0.399836729543542,-0.0129847676279312,
-1.54874256675859));
#8222=CARTESIAN_POINT('Ctrl Pts',(0.4,-0.00628514845714648,-1.55));
#8223=CARTESIAN_POINT('Ctrl Pts',(0.4,0.00628514845714648,-1.55));
#8224=CARTESIAN_POINT('Ctrl Pts',(0.399836729543542,0.0129847676279312,
-1.54874256675859));
#8225=CARTESIAN_POINT('Ctrl Pts',(0.399246581249293,0.0253018150396575,
-1.5436378293633));
#8226=CARTESIAN_POINT('Ctrl Pts',(0.398828027526425,0.0309197907817458,
-1.53979088733691));
#8227=CARTESIAN_POINT('Ctrl Pts',(0.398040841710914,0.0397909243921696,
-1.53091975372649));
#8228=CARTESIAN_POINT('Ctrl Pts',(0.397620851691571,0.0436378373878622,
-1.52530179409386));
#8229=CARTESIAN_POINT('Ctrl Pts',(0.397027412247524,0.0487425534891117,
-1.51298480122901));
#8230=CARTESIAN_POINT('Ctrl Pts',(0.396862696659689,0.05,-1.50628520096425));
#8231=CARTESIAN_POINT('Ctrl Pts',(0.396862696659689,0.05,-1.5));
#8232=CARTESIAN_POINT('',(1.2,-6.12323399573677E-18,-1.45));
#8233=CARTESIAN_POINT('',(-1.3,-6.12323399573677E-18,-1.45));
#8234=CARTESIAN_POINT('',(1.19895788082818,0.05,-1.5));
#8235=CARTESIAN_POINT('Ctrl Pts',(1.19895788082818,0.05,-1.5));
#8236=CARTESIAN_POINT('Ctrl Pts',(1.19895788082818,0.05,-1.50627889147831));
#8237=CARTESIAN_POINT('Ctrl Pts',(1.19901227819454,0.0487450133099081,-1.51297580462407));
#8238=CARTESIAN_POINT('Ctrl Pts',(1.19920885850753,0.0436421041657013,-1.52529455629072));
#8239=CARTESIAN_POINT('Ctrl Pts',(1.1993482149535,0.0397942217705328,-1.53091645634812));
#8240=CARTESIAN_POINT('Ctrl Pts',(1.19960989221221,0.0309164568000038,-1.53979422131865));
#8241=CARTESIAN_POINT('Ctrl Pts',(1.19974919586288,0.0252945565319674,-1.54364210404195));
#8242=CARTESIAN_POINT('Ctrl Pts',(1.19994565546462,0.0129758042228729,-1.54874501349991));
#8243=CARTESIAN_POINT('Ctrl Pts',(1.2,0.00627889083911038,-1.55));
#8244=CARTESIAN_POINT('Ctrl Pts',(1.2,-0.00627889083911041,-1.55));
#8245=CARTESIAN_POINT('Ctrl Pts',(1.19994565546462,-0.0129758042228729,
-1.54874501349991));
#8246=CARTESIAN_POINT('Ctrl Pts',(1.19974919586288,-0.0252945565319674,
-1.54364210404195));
#8247=CARTESIAN_POINT('Ctrl Pts',(1.19960989221221,-0.0309164568000038,
-1.53979422131865));
#8248=CARTESIAN_POINT('Ctrl Pts',(1.1993482149535,-0.0397942217705328,-1.53091645634812));
#8249=CARTESIAN_POINT('Ctrl Pts',(1.19920885850753,-0.0436421041657012,
-1.52529455629072));
#8250=CARTESIAN_POINT('Ctrl Pts',(1.19901227819454,-0.0487450133099081,
-1.51297580462407));
#8251=CARTESIAN_POINT('Ctrl Pts',(1.19895788082818,-0.05,-1.50627889147831));
#8252=CARTESIAN_POINT('Ctrl Pts',(1.19895788082818,-0.05,-1.49372110852169));
#8253=CARTESIAN_POINT('Ctrl Pts',(1.19901227819454,-0.0487450133099082,
-1.48702419537594));
#8254=CARTESIAN_POINT('Ctrl Pts',(1.19920885850753,-0.0436421041657014,
-1.47470544370928));
#8255=CARTESIAN_POINT('Ctrl Pts',(1.1993482149535,-0.0397942217705328,-1.46908354365188));
#8256=CARTESIAN_POINT('Ctrl Pts',(1.19960989221221,-0.0309164568000038,
-1.46020577868135));
#8257=CARTESIAN_POINT('Ctrl Pts',(1.19974919586288,-0.0252945565319675,
-1.45635789595805));
#8258=CARTESIAN_POINT('Ctrl Pts',(1.19994565546462,-0.0129758042228731,
-1.45125498650009));
#8259=CARTESIAN_POINT('Ctrl Pts',(1.2,-0.00627889083911039,-1.45));
#8260=CARTESIAN_POINT('Ctrl Pts',(1.2,9.10729824887824E-18,-1.45));
#8261=CARTESIAN_POINT('Ctrl Pts',(1.2,9.10729824887039E-18,-1.45));
#8262=CARTESIAN_POINT('Ctrl Pts',(1.2,0.00627889083911039,-1.45));
#8263=CARTESIAN_POINT('Ctrl Pts',(1.19994565546462,0.012975804222873,-1.45125498650009));
#8264=CARTESIAN_POINT('Ctrl Pts',(1.19974919586288,0.0252945565319674,-1.45635789595805));
#8265=CARTESIAN_POINT('Ctrl Pts',(1.19960989221221,0.0309164568000038,-1.46020577868135));
#8266=CARTESIAN_POINT('Ctrl Pts',(1.1993482149535,0.0397942217705329,-1.46908354365188));
#8267=CARTESIAN_POINT('Ctrl Pts',(1.19920885850753,0.0436421041657014,-1.47470544370928));
#8268=CARTESIAN_POINT('Ctrl Pts',(1.19901227819454,0.0487450133099082,-1.48702419537594));
#8269=CARTESIAN_POINT('Ctrl Pts',(1.19895788082818,0.05,-1.49372110852169));
#8270=CARTESIAN_POINT('Ctrl Pts',(1.19895788082818,0.05,-1.5));
#8271=CARTESIAN_POINT('Origin',(-1.3,0.,-0.5));
#8272=CARTESIAN_POINT('',(-1.19895788082818,0.05,-0.5));
#8273=CARTESIAN_POINT('',(-1.2,-6.12323399573677E-18,-0.45));
#8274=CARTESIAN_POINT('Ctrl Pts',(-1.19895788082818,0.05,-0.5));
#8275=CARTESIAN_POINT('Ctrl Pts',(-1.19895788082818,0.05,-0.493721108521693));
#8276=CARTESIAN_POINT('Ctrl Pts',(-1.19901227819454,0.0487450133099082,
-0.487024195375935));
#8277=CARTESIAN_POINT('Ctrl Pts',(-1.19920885850753,0.0436421041657014,
-0.47470544370928));
#8278=CARTESIAN_POINT('Ctrl Pts',(-1.1993482149535,0.0397942217705329,-0.469083543651878));
#8279=CARTESIAN_POINT('Ctrl Pts',(-1.19960989221221,0.0309164568000038,
-0.460205778681349));
#8280=CARTESIAN_POINT('Ctrl Pts',(-1.19974919586288,0.0252945565319675,
-0.456357895958046));
#8281=CARTESIAN_POINT('Ctrl Pts',(-1.19994565546462,0.012975804222873,-0.451254986500089));
#8282=CARTESIAN_POINT('Ctrl Pts',(-1.2,0.00627889083911039,-0.45));
#8283=CARTESIAN_POINT('Ctrl Pts',(-1.2,7.37257477290143E-18,-0.45));
#8284=CARTESIAN_POINT('',(-1.2,-8.08513827217387E-17,-0.55));
#8285=CARTESIAN_POINT('Ctrl Pts',(-1.2,-1.47451495458029E-17,-0.55));
#8286=CARTESIAN_POINT('Ctrl Pts',(-1.2,0.0062788908391104,-0.55));
#8287=CARTESIAN_POINT('Ctrl Pts',(-1.19994565546462,0.0129758042228731,
-0.548745013499911));
#8288=CARTESIAN_POINT('Ctrl Pts',(-1.19974919586288,0.0252945565319676,
-0.543642104041954));
#8289=CARTESIAN_POINT('Ctrl Pts',(-1.19960989221221,0.0309164568000038,
-0.539794221318651));
#8290=CARTESIAN_POINT('Ctrl Pts',(-1.1993482149535,0.0397942217705328,-0.530916456348121));
#8291=CARTESIAN_POINT('Ctrl Pts',(-1.19920885850753,0.0436421041657015,
-0.52529455629072));
#8292=CARTESIAN_POINT('Ctrl Pts',(-1.19901227819454,0.0487450133099082,
-0.512975804624065));
#8293=CARTESIAN_POINT('Ctrl Pts',(-1.19895788082818,0.05,-0.506278891478307));
#8294=CARTESIAN_POINT('Ctrl Pts',(-1.19895788082818,0.05,-0.5));
#8295=CARTESIAN_POINT('Ctrl Pts',(-1.2,7.37257477290143E-18,-0.45));
#8296=CARTESIAN_POINT('Ctrl Pts',(-1.2,-0.00627889083911038,-0.45));
#8297=CARTESIAN_POINT('Ctrl Pts',(-1.19994565546462,-0.012975804222873,
-0.451254986500089));
#8298=CARTESIAN_POINT('Ctrl Pts',(-1.19974919586288,-0.0252945565319675,
-0.456357895958046));
#8299=CARTESIAN_POINT('Ctrl Pts',(-1.19960989221221,-0.0309164568000038,
-0.460205778681349));
#8300=CARTESIAN_POINT('Ctrl Pts',(-1.1993482149535,-0.0397942217705328,
-0.469083543651878));
#8301=CARTESIAN_POINT('Ctrl Pts',(-1.19920885850753,-0.0436421041657014,
-0.47470544370928));
#8302=CARTESIAN_POINT('Ctrl Pts',(-1.19901227819454,-0.0487450133099082,
-0.487024195375935));
#8303=CARTESIAN_POINT('Ctrl Pts',(-1.19895788082818,-0.05,-0.493721108521693));
#8304=CARTESIAN_POINT('Ctrl Pts',(-1.19895788082818,-0.05,-0.506278891478307));
#8305=CARTESIAN_POINT('Ctrl Pts',(-1.19901227819454,-0.0487450133099082,
-0.512975804624065));
#8306=CARTESIAN_POINT('Ctrl Pts',(-1.19920885850753,-0.0436421041657015,
-0.52529455629072));
#8307=CARTESIAN_POINT('Ctrl Pts',(-1.1993482149535,-0.0397942217705328,
-0.530916456348121));
#8308=CARTESIAN_POINT('Ctrl Pts',(-1.19960989221221,-0.0309164568000039,
-0.539794221318651));
#8309=CARTESIAN_POINT('Ctrl Pts',(-1.19974919586288,-0.0252945565319676,
-0.543642104041954));
#8310=CARTESIAN_POINT('Ctrl Pts',(-1.19994565546462,-0.0129758042228732,
-0.548745013499911));
#8311=CARTESIAN_POINT('Ctrl Pts',(-1.2,-0.00627889083911043,-0.55));
#8312=CARTESIAN_POINT('Ctrl Pts',(-1.2,-1.4745149545795E-17,-0.55));
#8313=CARTESIAN_POINT('',(-0.4,-6.0973830808278E-18,-0.45));
#8314=CARTESIAN_POINT('',(-1.3,-6.12323399573677E-18,-0.45));
#8315=CARTESIAN_POINT('',(-0.4,-2.44929359829471E-17,-0.55));
#8316=CARTESIAN_POINT('Ctrl Pts',(-0.4,0.,-0.55));
#8317=CARTESIAN_POINT('Ctrl Pts',(-0.4,-0.00628514845714647,-0.55));
#8318=CARTESIAN_POINT('Ctrl Pts',(-0.399836729543542,-0.0129847676279313,
-0.548742566758595));
#8319=CARTESIAN_POINT('Ctrl Pts',(-0.399246581249293,-0.0253018150396576,
-0.543637829363298));
#8320=CARTESIAN_POINT('Ctrl Pts',(-0.398828027526425,-0.0309197907817458,
-0.539790887336909));
#8321=CARTESIAN_POINT('Ctrl Pts',(-0.398040841710914,-0.0397909243921697,
-0.530919753726485));
#8322=CARTESIAN_POINT('Ctrl Pts',(-0.397620851691571,-0.0436378373878619,
-0.525301794093861));
#8323=CARTESIAN_POINT('Ctrl Pts',(-0.397027412247524,-0.0487425534891115,
-0.512984801229014));
#8324=CARTESIAN_POINT('Ctrl Pts',(-0.396862696659689,-0.05,-0.506285200964255));
#8325=CARTESIAN_POINT('Ctrl Pts',(-0.396862696659689,-0.05,-0.493714799035745));
#8326=CARTESIAN_POINT('Ctrl Pts',(-0.397027412247524,-0.0487425534891115,
-0.487015198770986));
#8327=CARTESIAN_POINT('Ctrl Pts',(-0.397620851691571,-0.0436378373878619,
-0.474698205906139));
#8328=CARTESIAN_POINT('Ctrl Pts',(-0.398040841710914,-0.0397909243921697,
-0.469080246273515));
#8329=CARTESIAN_POINT('Ctrl Pts',(-0.398828027526425,-0.0309197907817458,
-0.460209112663091));
#8330=CARTESIAN_POINT('Ctrl Pts',(-0.399246581249293,-0.0253018150396576,
-0.456362170636702));
#8331=CARTESIAN_POINT('Ctrl Pts',(-0.399836729543542,-0.0129847676279313,
-0.451257433241405));
#8332=CARTESIAN_POINT('Ctrl Pts',(-0.4,-0.00628514845714648,-0.45));
#8333=CARTESIAN_POINT('Ctrl Pts',(-0.4,-6.07153216591882E-18,-0.45));
#8334=CARTESIAN_POINT('',(-0.396862696659689,0.05,-0.5));
#8335=CARTESIAN_POINT('Ctrl Pts',(-0.396862696659689,0.05,-0.5));
#8336=CARTESIAN_POINT('Ctrl Pts',(-0.396862696659689,0.05,-0.506285200964255));
#8337=CARTESIAN_POINT('Ctrl Pts',(-0.397027412247524,0.0487425534891115,
-0.512984801229014));
#8338=CARTESIAN_POINT('Ctrl Pts',(-0.397620851691571,0.0436378373878619,
-0.525301794093861));
#8339=CARTESIAN_POINT('Ctrl Pts',(-0.398040841710914,0.0397909243921697,
-0.530919753726485));
#8340=CARTESIAN_POINT('Ctrl Pts',(-0.398828027526425,0.0309197907817458,
-0.539790887336909));
#8341=CARTESIAN_POINT('Ctrl Pts',(-0.399246581249293,0.0253018150396576,
-0.543637829363298));
#8342=CARTESIAN_POINT('Ctrl Pts',(-0.399836729543542,0.0129847676279313,
-0.548742566758595));
#8343=CARTESIAN_POINT('Ctrl Pts',(-0.4,0.00628514845714647,-0.55));
#8344=CARTESIAN_POINT('Ctrl Pts',(-0.4,0.,-0.55));
#8345=CARTESIAN_POINT('Ctrl Pts',(-0.4,-6.07153216591882E-18,-0.45));
#8346=CARTESIAN_POINT('Ctrl Pts',(-0.4,0.00628514845714647,-0.45));
#8347=CARTESIAN_POINT('Ctrl Pts',(-0.399836729543542,0.0129847676279313,
-0.451257433241405));
#8348=CARTESIAN_POINT('Ctrl Pts',(-0.399246581249293,0.0253018150396577,
-0.456362170636702));
#8349=CARTESIAN_POINT('Ctrl Pts',(-0.398828027526425,0.0309197907817458,
-0.460209112663091));
#8350=CARTESIAN_POINT('Ctrl Pts',(-0.398040841710914,0.0397909243921697,
-0.469080246273515));
#8351=CARTESIAN_POINT('Ctrl Pts',(-0.397620851691571,0.0436378373878619,
-0.474698205906139));
#8352=CARTESIAN_POINT('Ctrl Pts',(-0.397027412247524,0.0487425534891115,
-0.487015198770986));
#8353=CARTESIAN_POINT('Ctrl Pts',(-0.396862696659689,0.05,-0.493714799035745));
#8354=CARTESIAN_POINT('Ctrl Pts',(-0.396862696659689,0.05,-0.5));
#8355=CARTESIAN_POINT('Origin',(-1.3,0.,-0.5));
#8356=CARTESIAN_POINT('',(0.396862696659689,0.05,-0.5));
#8357=CARTESIAN_POINT('',(0.4,-6.3142235153249E-18,-0.45));
#8358=CARTESIAN_POINT('Ctrl Pts',(0.396862696659689,0.05,-0.5));
#8359=CARTESIAN_POINT('Ctrl Pts',(0.396862696659689,0.05,-0.493714799035745));
#8360=CARTESIAN_POINT('Ctrl Pts',(0.397027412247524,0.0487425534891115,
-0.487015198770986));
#8361=CARTESIAN_POINT('Ctrl Pts',(0.397620851691571,0.0436378373878619,
-0.474698205906139));
#8362=CARTESIAN_POINT('Ctrl Pts',(0.398040841710914,0.0397909243921697,
-0.469080246273515));
#8363=CARTESIAN_POINT('Ctrl Pts',(0.398828027526425,0.0309197907817458,
-0.460209112663091));
#8364=CARTESIAN_POINT('Ctrl Pts',(0.399246581249293,0.0253018150396576,
-0.456362170636702));
#8365=CARTESIAN_POINT('Ctrl Pts',(0.399836729543542,0.0129847676279312,
-0.451257433241405));
#8366=CARTESIAN_POINT('Ctrl Pts',(0.4,0.00628514845714647,-0.45));
#8367=CARTESIAN_POINT('Ctrl Pts',(0.4,-6.50521303491303E-18,-0.45));
#8368=CARTESIAN_POINT('Ctrl Pts',(0.4,-6.50521303491303E-18,-0.45));
#8369=CARTESIAN_POINT('Ctrl Pts',(0.4,-0.00628514845714648,-0.45));
#8370=CARTESIAN_POINT('Ctrl Pts',(0.399836729543542,-0.0129847676279313,
-0.451257433241405));
#8371=CARTESIAN_POINT('Ctrl Pts',(0.399246581249293,-0.0253018150396576,
-0.456362170636702));
#8372=CARTESIAN_POINT('Ctrl Pts',(0.398828027526425,-0.0309197907817458,
-0.460209112663091));
#8373=CARTESIAN_POINT('Ctrl Pts',(0.398040841710914,-0.0397909243921697,
-0.469080246273515));
#8374=CARTESIAN_POINT('Ctrl Pts',(0.397620851691571,-0.0436378373878619,
-0.474698205906139));
#8375=CARTESIAN_POINT('Ctrl Pts',(0.397027412247524,-0.0487425534891115,
-0.487015198770986));
#8376=CARTESIAN_POINT('Ctrl Pts',(0.396862696659689,-0.05,-0.493714799035745));
#8377=CARTESIAN_POINT('Ctrl Pts',(0.396862696659689,-0.05,-0.506285200964255));
#8378=CARTESIAN_POINT('Ctrl Pts',(0.397027412247524,-0.0487425534891115,
-0.512984801229014));
#8379=CARTESIAN_POINT('Ctrl Pts',(0.397620851691571,-0.0436378373878619,
-0.525301794093861));
#8380=CARTESIAN_POINT('Ctrl Pts',(0.398040841710914,-0.0397909243921697,
-0.530919753726485));
#8381=CARTESIAN_POINT('Ctrl Pts',(0.398828027526425,-0.0309197907817458,
-0.539790887336909));
#8382=CARTESIAN_POINT('Ctrl Pts',(0.399246581249293,-0.0253018150396576,
-0.543637829363298));
#8383=CARTESIAN_POINT('Ctrl Pts',(0.399836729543542,-0.0129847676279313,
-0.548742566758595));
#8384=CARTESIAN_POINT('Ctrl Pts',(0.4,-0.00628514845714647,-0.55));
#8385=CARTESIAN_POINT('Ctrl Pts',(0.4,0.00628514845714647,-0.55));
#8386=CARTESIAN_POINT('Ctrl Pts',(0.399836729543542,0.0129847676279313,
-0.548742566758595));
#8387=CARTESIAN_POINT('Ctrl Pts',(0.399246581249293,0.0253018150396576,
-0.543637829363298));
#8388=CARTESIAN_POINT('Ctrl Pts',(0.398828027526425,0.0309197907817458,
-0.539790887336909));
#8389=CARTESIAN_POINT('Ctrl Pts',(0.398040841710914,0.0397909243921697,
-0.530919753726485));
#8390=CARTESIAN_POINT('Ctrl Pts',(0.397620851691571,0.043637837387862,-0.525301794093861));
#8391=CARTESIAN_POINT('Ctrl Pts',(0.397027412247524,0.0487425534891116,
-0.512984801229014));
#8392=CARTESIAN_POINT('Ctrl Pts',(0.396862696659689,0.05,-0.506285200964255));
#8393=CARTESIAN_POINT('Ctrl Pts',(0.396862696659689,0.05,-0.5));
#8394=CARTESIAN_POINT('',(1.2,-6.12323399573677E-18,-0.45));
#8395=CARTESIAN_POINT('',(-1.3,-6.12323399573677E-18,-0.45));
#8396=CARTESIAN_POINT('',(1.19895788082818,0.05,-0.5));
#8397=CARTESIAN_POINT('Ctrl Pts',(1.19895788082818,0.05,-0.5));
#8398=CARTESIAN_POINT('Ctrl Pts',(1.19895788082818,0.05,-0.506278891478307));
#8399=CARTESIAN_POINT('Ctrl Pts',(1.19901227819454,0.0487450133099082,-0.512975804624065));
#8400=CARTESIAN_POINT('Ctrl Pts',(1.19920885850753,0.0436421041657015,-0.52529455629072));
#8401=CARTESIAN_POINT('Ctrl Pts',(1.1993482149535,0.0397942217705328,-0.530916456348121));
#8402=CARTESIAN_POINT('Ctrl Pts',(1.19960989221221,0.0309164568000038,-0.539794221318651));
#8403=CARTESIAN_POINT('Ctrl Pts',(1.19974919586288,0.0252945565319676,-0.543642104041954));
#8404=CARTESIAN_POINT('Ctrl Pts',(1.19994565546462,0.0129758042228732,-0.548745013499911));
#8405=CARTESIAN_POINT('Ctrl Pts',(1.2,0.00627889083911041,-0.55));
#8406=CARTESIAN_POINT('Ctrl Pts',(1.2,-0.00627889083911043,-0.55));
#8407=CARTESIAN_POINT('Ctrl Pts',(1.19994565546462,-0.0129758042228732,
-0.548745013499911));
#8408=CARTESIAN_POINT('Ctrl Pts',(1.19974919586288,-0.0252945565319676,
-0.543642104041954));
#8409=CARTESIAN_POINT('Ctrl Pts',(1.19960989221221,-0.0309164568000039,
-0.539794221318651));
#8410=CARTESIAN_POINT('Ctrl Pts',(1.1993482149535,-0.0397942217705328,-0.530916456348121));
#8411=CARTESIAN_POINT('Ctrl Pts',(1.19920885850753,-0.0436421041657015,
-0.52529455629072));
#8412=CARTESIAN_POINT('Ctrl Pts',(1.19901227819454,-0.0487450133099082,
-0.512975804624065));
#8413=CARTESIAN_POINT('Ctrl Pts',(1.19895788082818,-0.05,-0.506278891478307));
#8414=CARTESIAN_POINT('Ctrl Pts',(1.19895788082818,-0.05,-0.493721108521693));
#8415=CARTESIAN_POINT('Ctrl Pts',(1.19901227819454,-0.0487450133099082,
-0.487024195375935));
#8416=CARTESIAN_POINT('Ctrl Pts',(1.19920885850753,-0.0436421041657014,
-0.47470544370928));
#8417=CARTESIAN_POINT('Ctrl Pts',(1.1993482149535,-0.0397942217705328,-0.469083543651878));
#8418=CARTESIAN_POINT('Ctrl Pts',(1.19960989221221,-0.0309164568000038,
-0.460205778681349));
#8419=CARTESIAN_POINT('Ctrl Pts',(1.19974919586288,-0.0252945565319675,
-0.456357895958046));
#8420=CARTESIAN_POINT('Ctrl Pts',(1.19994565546462,-0.012975804222873,-0.451254986500089));
#8421=CARTESIAN_POINT('Ctrl Pts',(1.2,-0.00627889083911039,-0.45));
#8422=CARTESIAN_POINT('Ctrl Pts',(1.2,3.90312782094782E-18,-0.45));
#8423=CARTESIAN_POINT('Ctrl Pts',(1.2,3.90312782093996E-18,-0.45));
#8424=CARTESIAN_POINT('Ctrl Pts',(1.2,0.00627889083911039,-0.45));
#8425=CARTESIAN_POINT('Ctrl Pts',(1.19994565546462,0.012975804222873,-0.451254986500089));
#8426=CARTESIAN_POINT('Ctrl Pts',(1.19974919586288,0.0252945565319675,-0.456357895958046));
#8427=CARTESIAN_POINT('Ctrl Pts',(1.19960989221221,0.0309164568000038,-0.460205778681349));
#8428=CARTESIAN_POINT('Ctrl Pts',(1.1993482149535,0.0397942217705329,-0.469083543651878));
#8429=CARTESIAN_POINT('Ctrl Pts',(1.19920885850753,0.0436421041657014,-0.47470544370928));
#8430=CARTESIAN_POINT('Ctrl Pts',(1.19901227819454,0.0487450133099082,-0.487024195375935));
#8431=CARTESIAN_POINT('Ctrl Pts',(1.19895788082818,0.05,-0.493721108521693));
#8432=CARTESIAN_POINT('Ctrl Pts',(1.19895788082818,0.05,-0.5));
#8433=CARTESIAN_POINT('Origin',(0.,0.,-3.2));
#8434=CARTESIAN_POINT('',(-0.4,-4.89858719658941E-17,-3.2));
#8435=CARTESIAN_POINT('Origin',(0.,0.,-3.2));
#8436=CARTESIAN_POINT('',(-0.4,-4.89858719658941E-17,-3.2));
#8437=CARTESIAN_POINT('',(-0.4,-4.89858719658941E-17,-3.2));
#8438=CARTESIAN_POINT('',(-0.4,-4.89858719658941E-17,-3.2));
#8439=CARTESIAN_POINT('',(-0.4,4.89858719658941E-17,1.4));
#8440=CARTESIAN_POINT('',(-0.4,-4.89858719658941E-17,-3.2));
#8441=CARTESIAN_POINT('Origin',(0.,0.,1.4));
#8442=CARTESIAN_POINT('Origin',(0.,0.,-3.2));
#8443=CARTESIAN_POINT('Origin',(0.,0.,-0.3));
#8444=CARTESIAN_POINT('',(-0.6185,-7.57444045272638E-17,1.4));
#8445=CARTESIAN_POINT('Origin',(0.,0.,1.4));
#8446=CARTESIAN_POINT('',(-0.6185,-7.57444045272638E-17,-0.3));
#8447=CARTESIAN_POINT('',(-0.6185,-7.57444045272638E-17,-0.3));
#8448=CARTESIAN_POINT('Origin',(0.,0.,-0.3));
#8449=CARTESIAN_POINT('Origin',(0.,0.,1.4));
#8450=CARTESIAN_POINT('Origin',(0.,0.,-3.5));
#8451=CARTESIAN_POINT('',(-1.2,-1.46957615897682E-16,-0.3));
#8452=CARTESIAN_POINT('Origin',(0.,0.,-0.3));
#8453=CARTESIAN_POINT('',(-1.2,-1.46957615897682E-16,-3.5));
#8454=CARTESIAN_POINT('',(-1.2,-1.46957615897682E-16,-3.5));
#8455=CARTESIAN_POINT('',(-1.2,-1.46957615897682E-16,-3.5));
#8456=CARTESIAN_POINT('',(-1.2,-1.46957615897682E-16,-3.5));
#8457=CARTESIAN_POINT('',(-1.2,-1.46957615897682E-16,-3.5));
#8458=CARTESIAN_POINT('Origin',(0.,0.,-3.5));
#8459=CARTESIAN_POINT('Origin',(0.,0.,-0.3));
#8460=CARTESIAN_POINT('Origin',(0.,0.,-3.5));
#8461=CARTESIAN_POINT('',(0.,0.,0.));
#8462=CARTESIAN_POINT('Origin',(0.,-5.2,2.9));
#8463=CARTESIAN_POINT('',(-2.,-5.2,2.9));
#8464=CARTESIAN_POINT('Origin',(0.,-5.2,2.9));
#8465=CARTESIAN_POINT('',(-0.685,-5.2,2.9));
#8466=CARTESIAN_POINT('Origin',(0.,-5.2,2.9));
#8467=CARTESIAN_POINT('Origin',(0.,-6.5,2.9));
#8468=CARTESIAN_POINT('',(-2.,-6.5,2.9));
#8469=CARTESIAN_POINT('',(-2.,-6.5,2.9));
#8470=CARTESIAN_POINT('Origin',(0.,-6.5,2.9));
#8471=CARTESIAN_POINT('Origin',(0.,-6.5,2.9));
#8472=CARTESIAN_POINT('Origin',(0.,-5.2,2.9));
#8473=CARTESIAN_POINT('',(-0.685,-3.6,2.9));
#8474=CARTESIAN_POINT('Origin',(0.,-3.6,2.9));
#8475=CARTESIAN_POINT('',(-0.685,-5.2,2.9));
#8476=CARTESIAN_POINT('Origin',(0.,-3.6,2.9));
#8477=CARTESIAN_POINT('Origin',(0.,-6.7,2.9));
#8478=CARTESIAN_POINT('',(-1.9,-6.5,2.9));
#8479=CARTESIAN_POINT('Origin',(0.,-6.5,2.9));
#8480=CARTESIAN_POINT('',(-1.9,-6.7,2.9));
#8481=CARTESIAN_POINT('',(-1.9,-6.7,2.9));
#8482=CARTESIAN_POINT('Origin',(0.,-6.7,2.9));
#8483=CARTESIAN_POINT('Origin',(0.,-6.5,2.9));
#8484=CARTESIAN_POINT('Origin',(0.,-6.7,2.9));
#8485=CARTESIAN_POINT('Origin',(-0.1,-6.8,1.9));
#8486=CARTESIAN_POINT('',(-0.1,-6.8,3.7));
#8487=CARTESIAN_POINT('',(-0.1,-6.8,1.9));
#8488=CARTESIAN_POINT('',(-0.1,-6.8,3.7));
#8489=CARTESIAN_POINT('',(-0.1,-6.7,3.7));
#8490=CARTESIAN_POINT('',(-0.1,-6.8,3.7));
#8491=CARTESIAN_POINT('',(-0.1,-6.7,1.9));
#8492=CARTESIAN_POINT('',(-0.1,-6.7,3.7));
#8493=CARTESIAN_POINT('',(-0.1,-6.8,1.9));
#8494=CARTESIAN_POINT('Origin',(0.1,-6.8,1.9));
#8495=CARTESIAN_POINT('',(0.1,-6.8,1.9));
#8496=CARTESIAN_POINT('',(-0.1,-6.8,1.9));
#8497=CARTESIAN_POINT('',(0.1,-6.7,1.9));
#8498=CARTESIAN_POINT('',(-0.1,-6.7,1.9));
#8499=CARTESIAN_POINT('',(0.1,-6.8,1.9));
#8500=CARTESIAN_POINT('Origin',(0.1,-6.8,3.7));
#8501=CARTESIAN_POINT('',(0.1,-6.8,3.7));
#8502=CARTESIAN_POINT('',(0.1,-6.8,1.9));
#8503=CARTESIAN_POINT('',(0.1,-6.7,3.7));
#8504=CARTESIAN_POINT('',(0.1,-6.7,1.9));
#8505=CARTESIAN_POINT('',(0.1,-6.8,3.7));
#8506=CARTESIAN_POINT('Origin',(0.,-6.8,4.3));
#8507=CARTESIAN_POINT('',(0.,-6.8,4.3));
#8508=CARTESIAN_POINT('',(0.1,-6.8,3.7));
#8509=CARTESIAN_POINT('',(0.,-6.7,4.3));
#8510=CARTESIAN_POINT('',(0.1,-6.7,3.7));
#8511=CARTESIAN_POINT('',(0.,-6.8,4.3));
#8512=CARTESIAN_POINT('Origin',(-0.1,-6.8,3.7));
#8513=CARTESIAN_POINT('',(0.,-6.8,4.3));
#8514=CARTESIAN_POINT('',(0.,-6.7,4.3));
#8515=CARTESIAN_POINT('Origin',(0.,-6.7,3.1));
#8516=CARTESIAN_POINT('Origin',(0.,-6.8,3.1));
#8517=CARTESIAN_POINT('',(0.,0.,0.));
#8518=CARTESIAN_POINT('Origin',(-4.,0.,-0.1));
#8519=CARTESIAN_POINT('',(-4.225,-2.75545529808155E-17,0.));
#8520=CARTESIAN_POINT('Origin',(-4.,0.,0.));
#8521=CARTESIAN_POINT('',(-4.225,2.75545529808155E-17,0.6));
#8522=CARTESIAN_POINT('',(-4.225,-2.75545529808155E-17,-0.1));
#8523=CARTESIAN_POINT('Origin',(-4.,0.,0.6));
#8524=CARTESIAN_POINT('Origin',(4.,0.,-0.1));
#8525=CARTESIAN_POINT('',(3.775,-2.75545529808154E-17,0.));
#8526=CARTESIAN_POINT('Origin',(4.,0.,0.));
#8527=CARTESIAN_POINT('',(3.775,2.75545529808154E-17,0.6));
#8528=CARTESIAN_POINT('',(3.775,-2.75545529808154E-17,-0.1));
#8529=CARTESIAN_POINT('Origin',(4.,0.,0.6));
#8530=CARTESIAN_POINT('Origin',(4.,5.4,-3.));
#8531=CARTESIAN_POINT('',(3.67,5.5,-3.));
#8532=CARTESIAN_POINT('Origin',(4.,5.5,-3.));
#8533=CARTESIAN_POINT('',(3.67,6.1,-3.));
#8534=CARTESIAN_POINT('',(3.67,5.4,-3.));
#8535=CARTESIAN_POINT('Origin',(4.,6.1,-3.));
#8536=CARTESIAN_POINT('Origin',(-4.,5.4,4.5));
#8537=CARTESIAN_POINT('',(-4.33,5.5,4.5));
#8538=CARTESIAN_POINT('Origin',(-4.,5.5,4.5));
#8539=CARTESIAN_POINT('',(-4.33,6.1,4.5));
#8540=CARTESIAN_POINT('',(-4.33,5.4,4.5));
#8541=CARTESIAN_POINT('Origin',(-4.,6.1,4.5));
#8542=CARTESIAN_POINT('Origin',(-4.,5.4,-3.));
#8543=CARTESIAN_POINT('',(-4.33,5.5,-3.));
#8544=CARTESIAN_POINT('Origin',(-4.,5.5,-3.));
#8545=CARTESIAN_POINT('',(-4.33,6.1,-3.));
#8546=CARTESIAN_POINT('',(-4.33,5.4,-3.));
#8547=CARTESIAN_POINT('Origin',(-4.,6.1,-3.));
#8548=CARTESIAN_POINT('Origin',(4.,5.4,4.5));
#8549=CARTESIAN_POINT('',(3.67,5.5,4.5));
#8550=CARTESIAN_POINT('Origin',(4.,5.5,4.5));
#8551=CARTESIAN_POINT('',(3.67,6.1,4.5));
#8552=CARTESIAN_POINT('',(3.67,5.4,4.5));
#8553=CARTESIAN_POINT('Origin',(4.,6.1,4.5));
#8554=CARTESIAN_POINT('Origin',(0.,5.5,1.));
#8555=CARTESIAN_POINT('',(5.,5.5,0.));
#8556=CARTESIAN_POINT('',(-5.,5.5,0.));
#8557=CARTESIAN_POINT('',(5.,5.5,0.));
#8558=CARTESIAN_POINT('',(-5.,5.5,-4.));
#8559=CARTESIAN_POINT('',(-5.,5.5,6.));
#8560=CARTESIAN_POINT('',(5.,5.5,-4.));
#8561=CARTESIAN_POINT('',(-5.,5.5,-4.));
#8562=CARTESIAN_POINT('',(5.,5.5,-4.));
#8563=CARTESIAN_POINT('Origin',(0.,5.5,1.));
#8564=CARTESIAN_POINT('',(5.,5.5,0.6));
#8565=CARTESIAN_POINT('',(-5.,5.5,0.6));
#8566=CARTESIAN_POINT('',(5.,5.5,0.6));
#8567=CARTESIAN_POINT('',(5.,5.5,6.));
#8568=CARTESIAN_POINT('',(5.,5.5,-4.));
#8569=CARTESIAN_POINT('',(-5.,5.5,6.));
#8570=CARTESIAN_POINT('',(5.,5.5,6.));
#8571=CARTESIAN_POINT('',(-5.,5.5,6.));
#8572=CARTESIAN_POINT('Origin',(5.,5.5,-4.));
#8573=CARTESIAN_POINT('',(-5.,6.1,-4.));
#8574=CARTESIAN_POINT('',(-5.,5.5,-4.));
#8575=CARTESIAN_POINT('',(5.,6.1,-4.));
#8576=CARTESIAN_POINT('',(-5.,6.1,-4.));
#8577=CARTESIAN_POINT('',(5.,5.5,-4.));
#8578=CARTESIAN_POINT('Origin',(-5.,5.5,6.));
#8579=CARTESIAN_POINT('',(5.,6.1,6.));
#8580=CARTESIAN_POINT('',(5.,5.5,6.));
#8581=CARTESIAN_POINT('',(-5.,6.1,6.));
#8582=CARTESIAN_POINT('',(5.,6.1,6.));
#8583=CARTESIAN_POINT('',(-5.,5.5,6.));
#8584=CARTESIAN_POINT('Origin',(0.,6.1,1.));
#8585=CARTESIAN_POINT('',(5.,6.1,-4.));
#8586=CARTESIAN_POINT('',(-5.,6.1,6.));
#8587=CARTESIAN_POINT('Origin',(0.,0.,-0.1));
#8588=CARTESIAN_POINT('',(-3.4,-4.163799117101E-16,0.));
#8589=CARTESIAN_POINT('Origin',(0.,0.,0.));
#8590=CARTESIAN_POINT('',(-3.4,4.163799117101E-16,0.6));
#8591=CARTESIAN_POINT('',(-3.4,-4.163799117101E-16,-0.1));
#8592=CARTESIAN_POINT('Origin',(0.,0.,0.6));
#8593=CARTESIAN_POINT('Origin',(5.,-4.5,0.));
#8594=CARTESIAN_POINT('',(5.,-4.5,0.));
#8595=CARTESIAN_POINT('',(5.,-4.5,0.));
#8596=CARTESIAN_POINT('',(5.,-4.5,0.6));
#8597=CARTESIAN_POINT('',(5.,-4.5,0.6));
#8598=CARTESIAN_POINT('',(5.,-4.5,0.));
#8599=CARTESIAN_POINT('Origin',(-5.,-4.5,0.));
#8600=CARTESIAN_POINT('',(-5.,-4.5,0.));
#8601=CARTESIAN_POINT('',(-5.,-4.5,0.));
#8602=CARTESIAN_POINT('',(-5.,-4.5,0.6));
#8603=CARTESIAN_POINT('',(-5.,-4.5,0.6));
#8604=CARTESIAN_POINT('',(-5.,-4.5,0.));
#8605=CARTESIAN_POINT('Origin',(-5.,5.5,0.));
#8606=CARTESIAN_POINT('',(-5.,5.5,0.));
#8607=CARTESIAN_POINT('',(-5.,5.5,0.6));
#8608=CARTESIAN_POINT('Origin',(0.,0.5,0.6));
#8609=CARTESIAN_POINT('Origin',(0.,0.5,0.));
#8610=CARTESIAN_POINT('',(0.,0.,0.));
#8611=CARTESIAN_POINT('Origin',(0.,-0.4,0.));
#8612=CARTESIAN_POINT('',(1.01036297108185,-0.4,0.));
#8613=CARTESIAN_POINT('',(0.505181485540923,-0.4,0.875));
#8614=CARTESIAN_POINT('',(0.505181485540923,-0.4,0.875));
#8615=CARTESIAN_POINT('',(-0.505181485540923,-0.4,0.875));
#8616=CARTESIAN_POINT('',(-0.505181485540923,-0.4,0.875));
#8617=CARTESIAN_POINT('',(-1.01036297108185,-0.4,-1.23733777851239E-16));
#8618=CARTESIAN_POINT('',(-1.01036297108185,-0.4,-1.23733777851239E-16));
#8619=CARTESIAN_POINT('',(-0.505181485540922,-0.4,-0.875));
#8620=CARTESIAN_POINT('',(-0.505181485540922,-0.4,-0.875));
#8621=CARTESIAN_POINT('',(0.505181485540923,-0.4,-0.875));
#8622=CARTESIAN_POINT('',(0.505181485540923,-0.4,-0.875));
#8623=CARTESIAN_POINT('',(1.01036297108185,-0.4,0.));
#8624=CARTESIAN_POINT('',(-0.685,-0.4,-8.38883057415937E-17));
#8625=CARTESIAN_POINT('Origin',(0.,-0.4,0.));
#8626=CARTESIAN_POINT('Origin',(0.,0.4,0.));
#8627=CARTESIAN_POINT('',(0.505181485540923,0.4,0.875));
#8628=CARTESIAN_POINT('',(1.01036297108185,0.4,0.));
#8629=CARTESIAN_POINT('',(0.505181485540923,0.4,0.875));
#8630=CARTESIAN_POINT('',(0.505181485540923,0.4,-0.875));
#8631=CARTESIAN_POINT('',(1.01036297108185,0.4,0.));
#8632=CARTESIAN_POINT('',(-0.505181485540922,0.4,-0.875));
#8633=CARTESIAN_POINT('',(0.505181485540923,0.4,-0.875));
#8634=CARTESIAN_POINT('',(-1.01036297108185,0.4,-1.23733777851239E-16));
#8635=CARTESIAN_POINT('',(-0.505181485540922,0.4,-0.875));
#8636=CARTESIAN_POINT('',(-0.505181485540923,0.4,0.875));
#8637=CARTESIAN_POINT('',(-1.01036297108185,0.4,-1.23733777851239E-16));
#8638=CARTESIAN_POINT('',(-0.505181485540923,0.4,0.875));
#8639=CARTESIAN_POINT('',(-0.685,0.4,8.38883057415937E-17));
#8640=CARTESIAN_POINT('Origin',(0.,0.4,0.));
#8641=CARTESIAN_POINT('Origin',(-0.505181485540923,0.,0.875));
#8642=CARTESIAN_POINT('',(0.505181485540923,0.,0.875));
#8643=CARTESIAN_POINT('',(-0.505181485540923,0.,0.875));
#8644=CARTESIAN_POINT('Origin',(-1.01036297108185,0.,-1.23733777851239E-16));
#8645=CARTESIAN_POINT('',(-1.01036297108185,0.,-1.23733777851239E-16));
#8646=CARTESIAN_POINT('Origin',(-0.505181485540922,0.,-0.875));
#8647=CARTESIAN_POINT('',(-0.505181485540922,0.,-0.875));
#8648=CARTESIAN_POINT('Origin',(0.505181485540923,0.,-0.875));
#8649=CARTESIAN_POINT('',(0.505181485540923,0.,-0.875));
#8650=CARTESIAN_POINT('Origin',(1.01036297108185,0.,0.));
#8651=CARTESIAN_POINT('',(1.01036297108185,0.,0.));
#8652=CARTESIAN_POINT('Origin',(0.505181485540923,0.,0.875));
#8653=CARTESIAN_POINT('Origin',(0.,0.,0.));
#8654=CARTESIAN_POINT('',(-0.685,1.82,-8.38883057415937E-17));
#8655=CARTESIAN_POINT('',(-0.685,0.,-8.38883057415937E-17));
#8656=CARTESIAN_POINT('Origin',(0.,1.82,0.));
#8657=CARTESIAN_POINT('Origin',(0.605,1.9,0.));
#8658=CARTESIAN_POINT('',(-0.605,1.9,-7.40911313484149E-17));
#8659=CARTESIAN_POINT('Origin',(0.,1.9,0.));
#8660=CARTESIAN_POINT('',(-0.46,1.9,-5.63337527607782E-17));
#8661=CARTESIAN_POINT('Origin',(0.,1.9,0.));
#8662=CARTESIAN_POINT('Origin',(0.,1.86,0.));
#8663=CARTESIAN_POINT('',(-0.645,1.86,-7.89897185450043E-17));
#8664=CARTESIAN_POINT('Origin',(0.,0.,0.));
#8665=CARTESIAN_POINT('',(-0.685,-1.82,-8.38883057415937E-17));
#8666=CARTESIAN_POINT('Origin',(0.,-1.82,0.));
#8667=CARTESIAN_POINT('',(-0.685,0.,-8.38883057415937E-17));
#8668=CARTESIAN_POINT('Origin',(0.,-1.86,0.));
#8669=CARTESIAN_POINT('',(-0.605,-1.9,-7.40911313484149E-17));
#8670=CARTESIAN_POINT('Origin',(0.,-1.9,0.));
#8671=CARTESIAN_POINT('',(-0.645,-1.86,-7.89897185450043E-17));
#8672=CARTESIAN_POINT('Origin',(0.46,-1.9,0.));
#8673=CARTESIAN_POINT('',(-0.46,-1.9,-5.63337527607782E-17));
#8674=CARTESIAN_POINT('Origin',(0.,-1.9,0.));
#8675=CARTESIAN_POINT('Origin',(0.,0.,0.));
#8676=CARTESIAN_POINT('',(-0.46,0.,-5.63337527607782E-17));
#8677=CARTESIAN_POINT('',(0.,0.,0.));
#8678=CARTESIAN_POINT('Origin',(0.,0.,2.4));
#8679=CARTESIAN_POINT('',(-0.2,-2.44929359829471E-17,3.2));
#8680=CARTESIAN_POINT('Origin',(0.,0.,3.2));
#8681=CARTESIAN_POINT('',(-0.2,-2.44929359829471E-17,2.4));
#8682=CARTESIAN_POINT('',(-0.2,-2.44929359829471E-17,2.4));
#8683=CARTESIAN_POINT('Origin',(0.,0.,2.4));
#8684=CARTESIAN_POINT('Origin',(0.,0.,2.4));
#8685=CARTESIAN_POINT('',(-0.6,-7.34788079488412E-17,3.2));
#8686=CARTESIAN_POINT('Origin',(0.,0.,3.2));
#8687=CARTESIAN_POINT('',(-0.6,-7.34788079488412E-17,2.4));
#8688=CARTESIAN_POINT('',(-0.6,-7.34788079488412E-17,2.4));
#8689=CARTESIAN_POINT('Origin',(0.,0.,2.4));
#8690=CARTESIAN_POINT('Origin',(0.,0.,3.2));
#8691=CARTESIAN_POINT('Origin',(0.,0.,2.4));
#8692=CARTESIAN_POINT('',(0.,0.,0.));
#8693=CARTESIAN_POINT('Origin',(0.,0.,5.3));
#8694=CARTESIAN_POINT('',(-0.4,-4.89858719658941E-17,5.3));
#8695=CARTESIAN_POINT('Origin',(0.,0.,5.3));
#8696=CARTESIAN_POINT('',(-0.15,1.83697019872103E-17,5.3));
#8697=CARTESIAN_POINT('Origin',(0.,0.,5.3));
#8698=CARTESIAN_POINT('Origin',(0.,0.,5.3));
#8699=CARTESIAN_POINT('',(-0.4,-4.89858719658941E-17,5.5));
#8700=CARTESIAN_POINT('Origin',(0.,0.,5.5));
#8701=CARTESIAN_POINT('',(-0.4,-4.89858719658941E-17,5.3));
#8702=CARTESIAN_POINT('Origin',(0.,0.,4.8));
#8703=CARTESIAN_POINT('',(-0.4,-4.89858719658941E-17,4.8));
#8704=CARTESIAN_POINT('Origin',(0.,0.,4.8));
#8705=CARTESIAN_POINT('',(-0.15,-1.83697019872103E-17,4.8));
#8706=CARTESIAN_POINT('Origin',(0.,0.,4.8));
#8707=CARTESIAN_POINT('Origin',(0.,0.,4.6));
#8708=CARTESIAN_POINT('',(-0.4,-4.89858719658941E-17,4.6));
#8709=CARTESIAN_POINT('Origin',(0.,0.,4.6));
#8710=CARTESIAN_POINT('',(-0.15,1.83697019872103E-17,4.6));
#8711=CARTESIAN_POINT('Origin',(0.,0.,4.6));
#8712=CARTESIAN_POINT('Origin',(0.,0.,4.6));
#8713=CARTESIAN_POINT('',(-0.4,-4.89858719658941E-17,4.6));
#8714=CARTESIAN_POINT('Origin',(0.,0.,2.4));
#8715=CARTESIAN_POINT('',(-0.15,-1.83697019872103E-17,2.4));
#8716=CARTESIAN_POINT('',(-0.15,-1.83697019872103E-17,2.4));
#8717=CARTESIAN_POINT('Origin',(0.,0.,2.4));
#8718=CARTESIAN_POINT('Origin',(0.,0.,2.4));
#8719=CARTESIAN_POINT('',(-0.15,-1.83697019872103E-17,2.4));
#8720=CARTESIAN_POINT('Origin',(0.,0.,5.5));
#8721=CARTESIAN_POINT('Origin',(0.,0.,2.2));
#8722=CARTESIAN_POINT('',(-0.4,-4.89858719658941E-17,2.4));
#8723=CARTESIAN_POINT('Origin',(0.,0.,2.4));
#8724=CARTESIAN_POINT('',(-0.4,-4.89858719658941E-17,1.9));
#8725=CARTESIAN_POINT('',(-0.4,-4.89858719658941E-17,2.2));
#8726=CARTESIAN_POINT('Origin',(0.,0.,1.9));
#8727=CARTESIAN_POINT('Origin',(0.,0.,2.4));
#8728=CARTESIAN_POINT('Origin',(0.,0.,1.9));
#8729=CARTESIAN_POINT('',(0.,0.,0.));
#8730=CARTESIAN_POINT('Origin',(0.,0.,4.8));
#8731=CARTESIAN_POINT('',(-0.16,-1.95943487863577E-17,5.));
#8732=CARTESIAN_POINT('Origin',(0.,0.,5.));
#8733=CARTESIAN_POINT('',(-0.16,-1.95943487863577E-17,4.8));
#8734=CARTESIAN_POINT('',(-0.16,-1.95943487863577E-17,4.8));
#8735=CARTESIAN_POINT('Origin',(0.,0.,4.8));
#8736=CARTESIAN_POINT('Origin',(0.,0.,4.8));
#8737=CARTESIAN_POINT('',(-2.2,-2.69422295812418E-16,5.));
#8738=CARTESIAN_POINT('Origin',(0.,0.,5.));
#8739=CARTESIAN_POINT('',(-2.2,-2.69422295812418E-16,4.8));
#8740=CARTESIAN_POINT('',(-2.2,-2.69422295812418E-16,4.8));
#8741=CARTESIAN_POINT('Origin',(0.,0.,4.8));
#8742=CARTESIAN_POINT('Origin',(0.,0.,5.));
#8743=CARTESIAN_POINT('Origin',(0.,0.,4.8));
#8744=CARTESIAN_POINT('',(0.,0.,0.));
#8745=CARTESIAN_POINT('Origin',(-6.2456986756515E-16,-3.4,4.9));
#8746=CARTESIAN_POINT('',(-0.275000000000001,-3.4,5.));
#8747=CARTESIAN_POINT('Origin',(-6.2456986756515E-16,-3.4,5.));
#8748=CARTESIAN_POINT('',(-0.275000000000001,-3.4,5.1));
#8749=CARTESIAN_POINT('',(-0.275000000000001,-3.4,4.9));
#8750=CARTESIAN_POINT('Origin',(-6.2456986756515E-16,-3.4,5.1));
#8751=CARTESIAN_POINT('Origin',(2.94448637286709,1.7,4.9));
#8752=CARTESIAN_POINT('',(2.66948637286709,1.7,5.));
#8753=CARTESIAN_POINT('Origin',(2.94448637286709,1.7,5.));
#8754=CARTESIAN_POINT('',(2.66948637286709,1.7,5.1));
#8755=CARTESIAN_POINT('',(2.66948637286709,1.7,4.9));
#8756=CARTESIAN_POINT('Origin',(2.94448637286709,1.7,5.1));
#8757=CARTESIAN_POINT('Origin',(2.0818995585505E-16,3.4,4.9));
#8758=CARTESIAN_POINT('',(-0.275,3.4,5.));
#8759=CARTESIAN_POINT('Origin',(2.0818995585505E-16,3.4,5.));
#8760=CARTESIAN_POINT('',(-0.275,3.4,5.1));
#8761=CARTESIAN_POINT('',(-0.275,3.4,4.9));
#8762=CARTESIAN_POINT('Origin',(2.0818995585505E-16,3.4,5.1));
#8763=CARTESIAN_POINT('Origin',(-2.94448637286709,1.7,4.9));
#8764=CARTESIAN_POINT('',(-3.21948637286709,1.7,5.));
#8765=CARTESIAN_POINT('Origin',(-2.94448637286709,1.7,5.));
#8766=CARTESIAN_POINT('',(-3.21948637286709,1.7,5.1));
#8767=CARTESIAN_POINT('',(-3.21948637286709,1.7,4.9));
#8768=CARTESIAN_POINT('Origin',(-2.94448637286709,1.7,5.1));
#8769=CARTESIAN_POINT('Origin',(-2.94448637286709,-1.7,4.9));
#8770=CARTESIAN_POINT('',(-3.21948637286709,-1.7,5.));
#8771=CARTESIAN_POINT('Origin',(-2.94448637286709,-1.7,5.));
#8772=CARTESIAN_POINT('',(-3.21948637286709,-1.7,5.1));
#8773=CARTESIAN_POINT('',(-3.21948637286709,-1.7,4.9));
#8774=CARTESIAN_POINT('Origin',(-2.94448637286709,-1.7,5.1));
#8775=CARTESIAN_POINT('Origin',(2.94448637286709,-1.7,4.9));
#8776=CARTESIAN_POINT('',(2.66948637286709,-1.7,5.));
#8777=CARTESIAN_POINT('Origin',(2.94448637286709,-1.7,5.));
#8778=CARTESIAN_POINT('',(2.66948637286709,-1.7,5.1));
#8779=CARTESIAN_POINT('',(2.66948637286709,-1.7,4.9));
#8780=CARTESIAN_POINT('Origin',(2.94448637286709,-1.7,5.1));
#8781=CARTESIAN_POINT('Origin',(0.,0.,5.));
#8782=CARTESIAN_POINT('',(-0.16,-1.95943487863577E-17,5.1));
#8783=CARTESIAN_POINT('Origin',(0.,0.,5.1));
#8784=CARTESIAN_POINT('',(-0.16,-1.95943487863577E-17,5.));
#8785=CARTESIAN_POINT('',(-0.16,-1.95943487863577E-17,5.));
#8786=CARTESIAN_POINT('Origin',(0.,0.,5.));
#8787=CARTESIAN_POINT('Origin',(0.,0.,5.));
#8788=CARTESIAN_POINT('',(-4.,-4.89858719658941E-16,5.1));
#8789=CARTESIAN_POINT('Origin',(0.,0.,5.1));
#8790=CARTESIAN_POINT('',(-4.,-4.89858719658941E-16,5.));
#8791=CARTESIAN_POINT('',(-4.,-4.89858719658941E-16,5.));
#8792=CARTESIAN_POINT('Origin',(0.,0.,5.));
#8793=CARTESIAN_POINT('Origin',(0.,0.,5.1));
#8794=CARTESIAN_POINT('Origin',(0.,0.,5.));
#8795=CARTESIAN_POINT('',(0.,0.,0.));
#8796=CARTESIAN_POINT('Origin',(0.,0.,5.3));
#8797=CARTESIAN_POINT('',(-0.41,-5.02105187650415E-17,5.7));
#8798=CARTESIAN_POINT('Origin',(0.,0.,5.7));
#8799=CARTESIAN_POINT('',(-0.41,-5.02105187650415E-17,5.3));
#8800=CARTESIAN_POINT('',(-0.41,-5.02105187650415E-17,5.3));
#8801=CARTESIAN_POINT('Origin',(0.,0.,5.3));
#8802=CARTESIAN_POINT('Origin',(0.,0.,5.3));
#8803=CARTESIAN_POINT('',(-0.6,-7.34788079488412E-17,5.7));
#8804=CARTESIAN_POINT('Origin',(0.,0.,5.7));
#8805=CARTESIAN_POINT('',(-0.6,-7.34788079488412E-17,5.3));
#8806=CARTESIAN_POINT('',(-0.6,-7.34788079488412E-17,5.3));
#8807=CARTESIAN_POINT('Origin',(0.,0.,5.3));
#8808=CARTESIAN_POINT('Origin',(0.,0.,5.7));
#8809=CARTESIAN_POINT('Origin',(0.,0.,5.3));
#8810=CARTESIAN_POINT('',(-2.2,-2.69422295812418E-16,5.3));
#8811=CARTESIAN_POINT('Origin',(0.,0.,5.3));
#8812=CARTESIAN_POINT('Origin',(0.,0.,5.1));
#8813=CARTESIAN_POINT('',(-0.16,-1.95943487863577E-17,5.3));
#8814=CARTESIAN_POINT('Origin',(0.,0.,5.3));
#8815=CARTESIAN_POINT('',(-0.16,-1.95943487863577E-17,5.1));
#8816=CARTESIAN_POINT('',(-0.16,-1.95943487863577E-17,5.1));
#8817=CARTESIAN_POINT('Origin',(0.,0.,5.1));
#8818=CARTESIAN_POINT('Origin',(0.,0.,5.1));
#8819=CARTESIAN_POINT('',(-2.2,-2.69422295812418E-16,5.1));
#8820=CARTESIAN_POINT('',(-2.2,-2.69422295812418E-16,5.1));
#8821=CARTESIAN_POINT('Origin',(0.,0.,5.1));
#8822=CARTESIAN_POINT('Origin',(0.,0.,5.3));
#8823=CARTESIAN_POINT('Origin',(0.,0.,5.1));
#8824=CARTESIAN_POINT('',(0.,0.,0.));
#8825=CARTESIAN_POINT('Origin',(-6.66133814775094E-16,-3.4,6.5));
#8826=CARTESIAN_POINT('',(-0.318956006072959,-2.98299632352941,6.5));
#8827=CARTESIAN_POINT('',(0.318956006072958,-2.98299632352941,6.5));
#8828=CARTESIAN_POINT('Origin',(0.,0.,6.5));
#8829=CARTESIAN_POINT('Origin',(-6.2456986756515E-16,-3.4,6.5));
#8830=CARTESIAN_POINT('Origin',(-6.2456986756515E-16,-3.4,5.7));
#8831=CARTESIAN_POINT('',(-0.318956006072959,-2.98299632352941,5.7));
#8832=CARTESIAN_POINT('',(-0.318956006072959,-2.98299632352941,5.7));
#8833=CARTESIAN_POINT('',(0.318956006072958,-2.98299632352941,5.7));
#8834=CARTESIAN_POINT('Origin',(-6.2456986756515E-16,-3.4,5.7));
#8835=CARTESIAN_POINT('',(0.318956006072958,-2.98299632352941,5.7));
#8836=CARTESIAN_POINT('Origin',(2.94448637286709,1.7,5.7));
#8837=CARTESIAN_POINT('',(2.42387259253558,1.76772216571351,6.5));
#8838=CARTESIAN_POINT('',(2.42387259253558,1.76772216571351,5.7));
#8839=CARTESIAN_POINT('',(2.42387259253558,1.76772216571351,5.7));
#8840=CARTESIAN_POINT('',(2.74282859860853,1.2152741578159,6.5));
#8841=CARTESIAN_POINT('Origin',(2.94448637286709,1.7,6.5));
#8842=CARTESIAN_POINT('',(2.74282859860853,1.2152741578159,5.7));
#8843=CARTESIAN_POINT('',(2.74282859860853,1.2152741578159,5.7));
#8844=CARTESIAN_POINT('Origin',(2.94448637286709,1.7,5.7));
#8845=CARTESIAN_POINT('Origin',(2.94448637286709,1.7,6.5));
#8846=CARTESIAN_POINT('Origin',(0.,0.,6.5));
#8847=CARTESIAN_POINT('Origin',(2.22044604925031E-16,3.4,6.5));
#8848=CARTESIAN_POINT('',(0.318956006072958,2.98299632352941,6.5));
#8849=CARTESIAN_POINT('',(-0.318956006072958,2.98299632352941,6.5));
#8850=CARTESIAN_POINT('Origin',(0.,0.,6.5));
#8851=CARTESIAN_POINT('Origin',(2.0818995585505E-16,3.4,6.5));
#8852=CARTESIAN_POINT('Origin',(2.0818995585505E-16,3.4,5.7));
#8853=CARTESIAN_POINT('',(0.318956006072958,2.98299632352941,5.7));
#8854=CARTESIAN_POINT('',(0.318956006072958,2.98299632352941,5.7));
#8855=CARTESIAN_POINT('',(-0.318956006072958,2.98299632352941,5.7));
#8856=CARTESIAN_POINT('Origin',(2.0818995585505E-16,3.4,5.7));
#8857=CARTESIAN_POINT('',(-0.318956006072958,2.98299632352941,5.7));
#8858=CARTESIAN_POINT('Origin',(-2.94448637286709,1.7,6.5));
#8859=CARTESIAN_POINT('',(-2.42387259253558,1.76772216571351,6.5));
#8860=CARTESIAN_POINT('',(-2.74282859860853,1.2152741578159,6.5));
#8861=CARTESIAN_POINT('Origin',(0.,0.,6.5));
#8862=CARTESIAN_POINT('Origin',(-2.94448637286709,1.7,6.5));
#8863=CARTESIAN_POINT('Origin',(-2.94448637286709,1.7,5.7));
#8864=CARTESIAN_POINT('',(-2.42387259253558,1.76772216571351,5.7));
#8865=CARTESIAN_POINT('',(-2.42387259253558,1.76772216571351,5.7));
#8866=CARTESIAN_POINT('',(-2.74282859860853,1.2152741578159,5.7));
#8867=CARTESIAN_POINT('Origin',(-2.94448637286709,1.7,5.7));
#8868=CARTESIAN_POINT('',(-2.74282859860853,1.2152741578159,5.7));
#8869=CARTESIAN_POINT('Origin',(-2.94448637286709,-1.7,6.5));
#8870=CARTESIAN_POINT('',(-2.74282859860853,-1.2152741578159,6.5));
#8871=CARTESIAN_POINT('',(-2.42387259253558,-1.76772216571351,6.5));
#8872=CARTESIAN_POINT('Origin',(0.,0.,6.5));
#8873=CARTESIAN_POINT('Origin',(-2.94448637286709,-1.7,6.5));
#8874=CARTESIAN_POINT('Origin',(-2.94448637286709,-1.7,5.7));
#8875=CARTESIAN_POINT('',(-2.74282859860853,-1.2152741578159,5.7));
#8876=CARTESIAN_POINT('',(-2.74282859860853,-1.2152741578159,5.7));
#8877=CARTESIAN_POINT('',(-2.42387259253558,-1.76772216571351,5.7));
#8878=CARTESIAN_POINT('Origin',(-2.94448637286709,-1.7,5.7));
#8879=CARTESIAN_POINT('',(-2.42387259253558,-1.76772216571351,5.7));
#8880=CARTESIAN_POINT('Origin',(2.94448637286709,-1.7,5.7));
#8881=CARTESIAN_POINT('',(2.74282859860853,-1.2152741578159,6.5));
#8882=CARTESIAN_POINT('',(2.74282859860853,-1.2152741578159,5.7));
#8883=CARTESIAN_POINT('',(2.74282859860853,-1.2152741578159,5.7));
#8884=CARTESIAN_POINT('',(2.42387259253558,-1.76772216571351,6.5));
#8885=CARTESIAN_POINT('Origin',(2.94448637286709,-1.7,6.5));
#8886=CARTESIAN_POINT('',(2.42387259253558,-1.76772216571351,5.7));
#8887=CARTESIAN_POINT('',(2.42387259253558,-1.76772216571351,5.7));
#8888=CARTESIAN_POINT('Origin',(2.94448637286709,-1.7,5.7));
#8889=CARTESIAN_POINT('Origin',(2.94448637286709,-1.7,6.5));
#8890=CARTESIAN_POINT('Origin',(0.,0.,6.5));
#8891=CARTESIAN_POINT('Origin',(0.,0.,5.7));
#8892=CARTESIAN_POINT('',(-3.,-3.67394039744206E-16,9.5));
#8893=CARTESIAN_POINT('Origin',(0.,0.,9.5));
#8894=CARTESIAN_POINT('',(-3.,-3.67394039744206E-16,5.7));
#8895=CARTESIAN_POINT('',(-3.,-3.67394039744206E-16,5.7));
#8896=CARTESIAN_POINT('Origin',(0.,0.,5.7));
#8897=CARTESIAN_POINT('Origin',(0.,0.,5.7));
#8898=CARTESIAN_POINT('Origin',(0.,0.,5.7));
#8899=CARTESIAN_POINT('Origin',(0.,0.,5.7));
#8900=CARTESIAN_POINT('Origin',(0.,0.,5.7));
#8901=CARTESIAN_POINT('Origin',(0.,0.,5.7));
#8902=CARTESIAN_POINT('Origin',(0.,0.,5.7));
#8903=CARTESIAN_POINT('Origin',(-6.2456986756515E-16,-3.4,4.9));
#8904=CARTESIAN_POINT('',(-0.275000000000001,-3.4,5.1));
#8905=CARTESIAN_POINT('Origin',(-6.2456986756515E-16,-3.4,5.1));
#8906=CARTESIAN_POINT('',(-0.275000000000001,-3.4,5.7));
#8907=CARTESIAN_POINT('',(-0.275000000000001,-3.4,4.9));
#8908=CARTESIAN_POINT('Origin',(-6.2456986756515E-16,-3.4,5.7));
#8909=CARTESIAN_POINT('Origin',(2.94448637286709,1.7,4.9));
#8910=CARTESIAN_POINT('',(2.66948637286709,1.7,5.1));
#8911=CARTESIAN_POINT('Origin',(2.94448637286709,1.7,5.1));
#8912=CARTESIAN_POINT('',(2.66948637286709,1.7,5.7));
#8913=CARTESIAN_POINT('',(2.66948637286709,1.7,4.9));
#8914=CARTESIAN_POINT('Origin',(2.94448637286709,1.7,5.7));
#8915=CARTESIAN_POINT('Origin',(2.0818995585505E-16,3.4,4.9));
#8916=CARTESIAN_POINT('',(-0.275,3.4,5.1));
#8917=CARTESIAN_POINT('Origin',(2.0818995585505E-16,3.4,5.1));
#8918=CARTESIAN_POINT('',(-0.275,3.4,5.7));
#8919=CARTESIAN_POINT('',(-0.275,3.4,4.9));
#8920=CARTESIAN_POINT('Origin',(2.0818995585505E-16,3.4,5.7));
#8921=CARTESIAN_POINT('Origin',(-2.94448637286709,1.7,4.9));
#8922=CARTESIAN_POINT('',(-3.21948637286709,1.7,5.1));
#8923=CARTESIAN_POINT('Origin',(-2.94448637286709,1.7,5.1));
#8924=CARTESIAN_POINT('',(-3.21948637286709,1.7,5.7));
#8925=CARTESIAN_POINT('',(-3.21948637286709,1.7,4.9));
#8926=CARTESIAN_POINT('Origin',(-2.94448637286709,1.7,5.7));
#8927=CARTESIAN_POINT('Origin',(-2.94448637286709,-1.7,4.9));
#8928=CARTESIAN_POINT('',(-3.21948637286709,-1.7,5.1));
#8929=CARTESIAN_POINT('Origin',(-2.94448637286709,-1.7,5.1));
#8930=CARTESIAN_POINT('',(-3.21948637286709,-1.7,5.7));
#8931=CARTESIAN_POINT('',(-3.21948637286709,-1.7,4.9));
#8932=CARTESIAN_POINT('Origin',(-2.94448637286709,-1.7,5.7));
#8933=CARTESIAN_POINT('Origin',(2.94448637286709,-1.7,4.9));
#8934=CARTESIAN_POINT('',(2.66948637286709,-1.7,5.1));
#8935=CARTESIAN_POINT('Origin',(2.94448637286709,-1.7,5.1));
#8936=CARTESIAN_POINT('',(2.66948637286709,-1.7,5.7));
#8937=CARTESIAN_POINT('',(2.66948637286709,-1.7,4.9));
#8938=CARTESIAN_POINT('Origin',(2.94448637286709,-1.7,5.7));
#8939=CARTESIAN_POINT('Origin',(0.,0.,8.7));
#8940=CARTESIAN_POINT('',(-0.34,-4.163799117101E-17,8.8));
#8941=CARTESIAN_POINT('Origin',(0.,0.,8.8));
#8942=CARTESIAN_POINT('',(-0.34,4.163799117101E-17,9.5));
#8943=CARTESIAN_POINT('',(-0.34,-4.163799117101E-17,8.7));
#8944=CARTESIAN_POINT('Origin',(0.,0.,9.5));
#8945=CARTESIAN_POINT('Origin',(0.,0.,5.));
#8946=CARTESIAN_POINT('',(-2.5,-3.06161699786838E-16,5.1));
#8947=CARTESIAN_POINT('Origin',(0.,0.,5.1));
#8948=CARTESIAN_POINT('',(-2.5,-3.06161699786838E-16,8.8));
#8949=CARTESIAN_POINT('',(-2.5,-3.06161699786838E-16,5.));
#8950=CARTESIAN_POINT('Origin',(0.,0.,8.8));
#8951=CARTESIAN_POINT('Origin',(0.,0.,8.8));
#8952=CARTESIAN_POINT('Origin',(0.,0.,9.5));
#8953=CARTESIAN_POINT('Origin',(0.,0.,5.1));
#8954=CARTESIAN_POINT('',(-4.,-4.89858719658941E-16,5.7));
#8955=CARTESIAN_POINT('Origin',(0.,0.,5.7));
#8956=CARTESIAN_POINT('',(-4.,-4.89858719658941E-16,5.1));
#8957=CARTESIAN_POINT('',(-4.,-4.89858719658941E-16,5.1));
#8958=CARTESIAN_POINT('Origin',(0.,0.,5.1));
#8959=CARTESIAN_POINT('Origin',(0.,0.,5.7));
#8960=CARTESIAN_POINT('Origin',(0.,0.,5.1));
#8961=CARTESIAN_POINT('',(0.,0.,0.));
#8962=CARTESIAN_POINT('Ctrl Pts',(0.799999065628721,0.00692558823944229,
5.30024010712383));
#8963=CARTESIAN_POINT('Ctrl Pts',(0.799974755250737,0.187114846749742,5.31274930893178));
#8964=CARTESIAN_POINT('Ctrl Pts',(0.674578200671659,0.546127076651831,5.33781512365923));
#8965=CARTESIAN_POINT('Ctrl Pts',(0.187998995393781,0.852903359039399,5.37564381521248));
#8966=CARTESIAN_POINT('Ctrl Pts',(-0.386721866921525,0.788448388841122,
5.41368605209984));
#8967=CARTESIAN_POINT('Ctrl Pts',(-0.7983994419892,0.377627224111744,5.45194644400096));
#8968=CARTESIAN_POINT('Ctrl Pts',(-0.864375113399524,-0.203617876612744,
5.49042055747836));
#8969=CARTESIAN_POINT('Ctrl Pts',(-0.552019639313923,-0.701812288635587,
5.52910737914477));
#8970=CARTESIAN_POINT('Ctrl Pts',(0.00615426428515267,-0.897757418326962,
5.56800374230524));
#8971=CARTESIAN_POINT('Ctrl Pts',(0.463089276607972,-0.737891299975203,
5.59986549204054));
#8972=CARTESIAN_POINT('Ctrl Pts',(0.706662565433678,-0.474149107376678,
5.62457829573124));
#8973=CARTESIAN_POINT('Ctrl Pts',(0.854347338563578,-0.169471123140589,
5.6478904398873));
#8974=CARTESIAN_POINT('Ctrl Pts',(0.854381411403854,0.269671075667267,5.67712918390586));
#8975=CARTESIAN_POINT('Ctrl Pts',(0.581578462406747,0.670744438556907,5.70943359497258));
#8976=CARTESIAN_POINT('Ctrl Pts',(0.189982000930166,0.858805851522918,5.73891161848027));
#8977=CARTESIAN_POINT('Ctrl Pts',(-0.201854620920769,0.859148371452269,
5.76552549972421));
#8978=CARTESIAN_POINT('Ctrl Pts',(-0.556170302204947,0.688486751453872,
5.79222147180784));
#8979=CARTESIAN_POINT('Ctrl Pts',(-0.802120584542054,0.380288702719923,
5.81899788702529));
#8980=CARTESIAN_POINT('Ctrl Pts',(-0.890321102734134,-0.0053444036833259,
5.84585301727138));
#8981=CARTESIAN_POINT('Ctrl Pts',(-0.816781798992104,-0.327577127496462,
5.86829638740099));
#8982=CARTESIAN_POINT('Ctrl Pts',(-0.678277859648778,-0.547664335405585,
5.88628859994389));
#8983=CARTESIAN_POINT('Ctrl Pts',(-0.494316135451619,-0.731945478665225,
5.90430550175064));
#8984=CARTESIAN_POINT('Ctrl Pts',(-0.194941007989142,-0.876310026230692,
5.92687230420244));
#8985=CARTESIAN_POINT('Ctrl Pts',(0.204945568353256,-0.876409485122255,
5.95402353339188));
#8986=CARTESIAN_POINT('Ctrl Pts',(0.566325487118899,-0.702556101088839,
5.98124373289334));
#8987=CARTESIAN_POINT('Ctrl Pts',(0.816751045229916,-0.388463305588866,
6.00853075028047));
#8988=CARTESIAN_POINT('Ctrl Pts',(0.917174982875959,0.0480250206861584,
6.03892142694837));
#8989=CARTESIAN_POINT('Ctrl Pts',(0.768829350780382,0.528866010776267,6.07244001895545));
#8990=CARTESIAN_POINT('Ctrl Pts',(0.338627495917749,0.872873034891815,6.10911095186911));
#8991=CARTESIAN_POINT('Ctrl Pts',(-0.212178222814091,0.914151313349766,
6.14588130840082));
#8992=CARTESIAN_POINT('Ctrl Pts',(-0.691759933067223,0.637451614256161,
6.18274515756461));
#8993=CARTESIAN_POINT('Ctrl Pts',(-0.932934482256533,0.137697594997002,
6.21969639210087));
#8994=CARTESIAN_POINT('Ctrl Pts',(-0.84730393945114,-0.435496308403701,
6.25827178793966));
#8995=CARTESIAN_POINT('Ctrl Pts',(-0.415273257958933,-0.868240176171726,
6.29847623644814));
#8996=CARTESIAN_POINT('Ctrl Pts',(0.146189896678077,-0.930950222024402,
6.33566388079779));
#8997=CARTESIAN_POINT('Ctrl Pts',(0.578787425776111,-0.722091726547751,
6.36825221458814));
#8998=CARTESIAN_POINT('Ctrl Pts',(0.835229259505866,-0.400278931762148,
6.3962159259868));
#8999=CARTESIAN_POINT('Ctrl Pts',(0.943177486850013,0.0688606453452641,
6.42887288667825));
#9000=CARTESIAN_POINT('Ctrl Pts',(0.756462512495389,0.604750444420971,6.46623690685835));
#9001=CARTESIAN_POINT('Ctrl Pts',(0.214509054547464,0.945343920852135,6.50831791566041));
#9002=CARTESIAN_POINT('Ctrl Pts',(-0.421585054233784,0.873670673138226,
6.55043539297339));
#9003=CARTESIAN_POINT('Ctrl Pts',(-0.874725713994987,0.420703846750279,
6.59257924943873));
#9004=CARTESIAN_POINT('Ctrl Pts',(-0.946491736933492,-0.216206220818672,
6.63473932973225));
#9005=CARTESIAN_POINT('Ctrl Pts',(-0.605472064685913,-0.758979181442101,
6.67690544450194));
#9006=CARTESIAN_POINT('Ctrl Pts',(-0.000509641250504898,-0.970641038681315,
6.71906739492544));
#9007=CARTESIAN_POINT('Ctrl Pts',(0.604236817182525,-0.758999928674301,
6.76121498571335));
#9008=CARTESIAN_POINT('Ctrl Pts',(0.944676427167983,-0.216670516455945,
6.80333805746961));
#9009=CARTESIAN_POINT('Ctrl Pts',(0.873719648783539,0.418956634979468,6.8454265042638));
#9010=CARTESIAN_POINT('Ctrl Pts',(0.421037273012308,0.871132652579719,6.88747029453994));
#9011=CARTESIAN_POINT('Ctrl Pts',(-0.142342851291253,0.933831870869633,
6.92479402146672));
#9012=CARTESIAN_POINT('Ctrl Pts',(-0.575104466317865,0.724476767443434,
6.95741054274359));
#9013=CARTESIAN_POINT('Ctrl Pts',(-0.831597121038275,0.403171008458228,
6.98533606563364));
#9014=CARTESIAN_POINT('Ctrl Pts',(-0.922808904665035,0.00254068286457492,
7.01322724854536));
#9015=CARTESIAN_POINT('Ctrl Pts',(-0.831484359832733,-0.397369041930912,
7.04108128388358));
#9016=CARTESIAN_POINT('Ctrl Pts',(-0.576024516479058,-0.717622866946566,
7.06889539860548));
#9017=CARTESIAN_POINT('Ctrl Pts',(-0.207464718971416,-0.895095126308869,
7.09666685370961));
#9018=CARTESIAN_POINT('Ctrl Pts',(0.200869050822812,-0.894893573965507,
7.12439296344474));
#9019=CARTESIAN_POINT('Ctrl Pts',(0.568135301656786,-0.717941543510051,
7.15207107099507));
#9020=CARTESIAN_POINT('Ctrl Pts',(0.821742493579341,-0.399813712939291,
7.17969857736332));
#9021=CARTESIAN_POINT('Ctrl Pts',(0.912100647381109,-0.00372699171446918,
7.20727292857109));
#9022=CARTESIAN_POINT('Ctrl Pts',(0.821667160899362,0.391120281113409,7.23479162069698));
#9023=CARTESIAN_POINT('Ctrl Pts',(0.527798142032111,0.760706416566583,7.26682897888736));
#9024=CARTESIAN_POINT('Ctrl Pts',(0.00437094025093319,0.944184514671381,
7.30334225024583));
#9025=CARTESIAN_POINT('Ctrl Pts',(-0.583164611559206,0.738086874931468,
7.3442757526392));
#9026=CARTESIAN_POINT('Ctrl Pts',(-0.912546668924433,0.213026529714121,
7.38505770065783));
#9027=CARTESIAN_POINT('Ctrl Pts',(-0.843060529623956,-0.400706652853849,
7.42568118182012));
#9028=CARTESIAN_POINT('Ctrl Pts',(-0.407835437985135,-0.835237258109269,
7.46613873367218));
#9029=CARTESIAN_POINT('Ctrl Pts',(0.200737244244076,-0.903598468057941,
7.5064251969444));
#9030=CARTESIAN_POINT('Ctrl Pts',(0.71672352100227,-0.578479045751934,7.54653146106904));
#9031=CARTESIAN_POINT('Ctrl Pts',(0.849917343436364,-0.197265324952655,
7.57314919120958));
#9032=CARTESIAN_POINT('Ctrl Pts',(0.849943147209423,-0.00600671278230411,
7.58642685605973));
#9033=CARTESIAN_POINT('Ctrl Pts',(0.770079135866838,0.00692155156817904,
5.30024010712383));
#9034=CARTESIAN_POINT('Ctrl Pts',(0.770055720112496,0.180479832525886,5.31228896941391));
#9035=CARTESIAN_POINT('Ctrl Pts',(0.649347137055222,0.526118956744516,5.33641790275693));
#9036=CARTESIAN_POINT('Ctrl Pts',(0.180677599950648,0.821679099419469,5.37285586761231));
#9037=CARTESIAN_POINT('Ctrl Pts',(-0.373128354027995,0.759596327571503,
5.40950951731212));
#9038=CARTESIAN_POINT('Ctrl Pts',(-0.770051450984494,0.363580245990391,
5.44639246645647));
#9039=CARTESIAN_POINT('Ctrl Pts',(-0.833750732775199,-0.197081341774288,
5.48350071817735));
#9040=CARTESIAN_POINT('Ctrl Pts',(-0.532331315046715,-0.677969641751496,
5.5208364575171));
#9041=CARTESIAN_POINT('Ctrl Pts',(0.00675318837749655,-0.867294541965757,
5.558400781988));
#9042=CARTESIAN_POINT('Ctrl Pts',(0.448424688054875,-0.712845112569316,
5.58919119813692));
#9043=CARTESIAN_POINT('Ctrl Pts',(0.684012778929899,-0.457765801730765,
5.61309167265538));
#9044=CARTESIAN_POINT('Ctrl Pts',(0.82691455168644,-0.162993811747473,5.6356443242608));
#9045=CARTESIAN_POINT('Ctrl Pts',(0.82699649983482,0.262124971545771,5.66394696022895));
#9046=CARTESIAN_POINT('Ctrl Pts',(0.562750276158912,0.650752034831193,5.69524212629919));
#9047=CARTESIAN_POINT('Ctrl Pts',(0.183080725565527,0.833119661747386,5.72381920452852));
#9048=CARTESIAN_POINT('Ctrl Pts',(-0.197084703463694,0.833490239824234,
5.74963623066415));
#9049=CARTESIAN_POINT('Ctrl Pts',(-0.541119975074503,0.667809968168665,
5.77555492059187));
#9050=CARTESIAN_POINT('Ctrl Pts',(-0.780113947482257,0.368392103745768,
5.80156649252668));
#9051=CARTESIAN_POINT('Ctrl Pts',(-0.865905134963049,-0.00656170868815412,
5.82767483842523));
#9052=CARTESIAN_POINT('Ctrl Pts',(-0.794375852743549,-0.320111204417347,
5.84950881094256));
#9053=CARTESIAN_POINT('Ctrl Pts',(-0.659521269028743,-0.534410811061921,
5.86702622272765));
#9054=CARTESIAN_POINT('Ctrl Pts',(-0.480335340635082,-0.713917263728105,
5.88457460840773));
#9055=CARTESIAN_POINT('Ctrl Pts',(-0.188587087034294,-0.854642083096481,
5.90656315000717));
#9056=CARTESIAN_POINT('Ctrl Pts',(0.201462529249485,-0.854779640403169,
5.9330427097564));
#9057=CARTESIAN_POINT('Ctrl Pts',(0.554262072476138,-0.685098200004362,
5.95961046024728));
#9058=CARTESIAN_POINT('Ctrl Pts',(0.798967352085236,-0.378235706832728,
5.98626742358202));
#9059=CARTESIAN_POINT('Ctrl Pts',(0.89721847916451,0.0485845903033819,6.01597993297972));
#9060=CARTESIAN_POINT('Ctrl Pts',(0.752070839701578,0.519313731169816,6.04878757680353));
#9061=CARTESIAN_POINT('Ctrl Pts',(0.330497979661169,0.856564661134425,6.08472490306161));
#9062=CARTESIAN_POINT('Ctrl Pts',(-0.209973066601811,0.897165035883339,
6.12079612560753));
#9063=CARTESIAN_POINT('Ctrl Pts',(-0.68120970786282,0.625397209779933,6.15700765884533));
#9064=CARTESIAN_POINT('Ctrl Pts',(-0.918572438612158,0.13378828614086,6.19335554838198));
#9065=CARTESIAN_POINT('Ctrl Pts',(-0.83433799028855,-0.430850802296383,
6.23134861625561));
#9066=CARTESIAN_POINT('Ctrl Pts',(-0.408316865658928,-0.857793214073537,
6.2709938323838));
#9067=CARTESIAN_POINT('Ctrl Pts',(0.146288162282126,-0.919868958459814,
6.30771962173879));
#9068=CARTESIAN_POINT('Ctrl Pts',(0.574223288772557,-0.71333190916663,6.33995134748923));
#9069=CARTESIAN_POINT('Ctrl Pts',(0.828161465810104,-0.394717048019018,
6.36763553346922));
#9070=CARTESIAN_POINT('Ctrl Pts',(0.935214831817973,0.0702367246280078,
6.39999872706231));
#9071=CARTESIAN_POINT('Ctrl Pts',(0.750063250540666,0.602049612066996,6.43706602732403));
#9072=CARTESIAN_POINT('Ctrl Pts',(0.211520380136952,0.940697836629915,6.47888152979277));
#9073=CARTESIAN_POINT('Ctrl Pts',(-0.421676436247289,0.869510362169926,
6.52079671898647));
#9074=CARTESIAN_POINT('Ctrl Pts',(-0.873553921061096,0.418039168812721,
6.56280406058959));
#9075=CARTESIAN_POINT('Ctrl Pts',(-0.945379508760524,-0.217899113421901,
6.60489250808515));
#9076=CARTESIAN_POINT('Ctrl Pts',(-0.604485708962148,-0.760787236561161,
6.64705240063428));
#9077=CARTESIAN_POINT('Ctrl Pts',(0.00138176225817566,-0.972945250150102,
6.6892731978663));
#9078=CARTESIAN_POINT('Ctrl Pts',(0.608080140735397,-0.760798630125154,
6.73154461863783));
#9079=CARTESIAN_POINT('Ctrl Pts',(0.950239792824421,-0.216025881173973,
6.77385551750453));
#9080=CARTESIAN_POINT('Ctrl Pts',(0.879017289772042,0.423590907490335,6.81620268596198));
#9081=CARTESIAN_POINT('Ctrl Pts',(0.422960901581898,0.879362908068112,6.85856017311708));
#9082=CARTESIAN_POINT('Ctrl Pts',(-0.145593093231334,0.942790559668914,
6.89621968364161));
#9083=CARTESIAN_POINT('Ctrl Pts',(-0.582932490358213,0.73127758858104,6.92917512678282));
#9084=CARTESIAN_POINT('Ctrl Pts',(-0.842401988544835,0.406320842666593,
6.957415448388));
#9085=CARTESIAN_POINT('Ctrl Pts',(-0.934795701286156,0.000685604828614038,
6.985653769321));
#9086=CARTESIAN_POINT('Ctrl Pts',(-0.842294766840471,-0.404603381671274,
7.01387715318084));
#9087=CARTESIAN_POINT('Ctrl Pts',(-0.583187447906784,-0.729494778082508,
7.04208836805485));
#9088=CARTESIAN_POINT('Ctrl Pts',(-0.20899792340701,-0.909726737101999,
7.07028057033796));
#9089=CARTESIAN_POINT('Ctrl Pts',(0.206012719667752,-0.909558569724805,
7.09845804612497));
#9090=CARTESIAN_POINT('Ctrl Pts',(0.579624839727756,-0.72959465407811,7.12660922044297));
#9091=CARTESIAN_POINT('Ctrl Pts',(0.837867106227739,-0.405711083857505,
7.15473493621397));
#9092=CARTESIAN_POINT('Ctrl Pts',(0.929983985732294,-0.00207542308664412,
7.18283200361311));
#9093=CARTESIAN_POINT('Ctrl Pts',(0.837775922394786,0.40066931879227,7.21089711007051));
#9094=CARTESIAN_POINT('Ctrl Pts',(0.537807840870324,0.777996358577212,7.24360025784798));
#9095=CARTESIAN_POINT('Ctrl Pts',(0.00294143852372089,0.965597941956312,
7.28090792189502));
#9096=CARTESIAN_POINT('Ctrl Pts',(-0.59827790503141,0.754837569025208,7.32278668150169));
#9097=CARTESIAN_POINT('Ctrl Pts',(-0.935814946990508,0.217001877726337,
7.36456027598379));
#9098=CARTESIAN_POINT('Ctrl Pts',(-0.864667175323564,-0.412475523451113,
7.40622093849563));
#9099=CARTESIAN_POINT('Ctrl Pts',(-0.417866766747618,-0.858729006758795,
7.44775776125507));
#9100=CARTESIAN_POINT('Ctrl Pts',(0.207655975088153,-0.929085997388315,
7.48916462895728));
#9101=CARTESIAN_POINT('Ctrl Pts',(0.73862266392267,-0.594662305466805,7.53042707168622));
#9102=CARTESIAN_POINT('Ctrl Pts',(0.875837799539084,-0.201989676969171,
7.55784229424685));
#9103=CARTESIAN_POINT('Ctrl Pts',(0.875864379853922,-0.00497530564290791,
7.5715195387037));
#9104=CARTESIAN_POINT('Ctrl Pts',(0.710428941733949,0.00492953088558486,
5.32881831830437));
#9105=CARTESIAN_POINT('Ctrl Pts',(0.71040731614315,0.165219065394011,5.33994603008611));
#9106=CARTESIAN_POINT('Ctrl Pts',(0.599024128589712,0.483870366740507,5.3621924509196));
#9107=CARTESIAN_POINT('Ctrl Pts',(0.167205166996449,0.75612127364975,5.39576440291455));
#9108=CARTESIAN_POINT('Ctrl Pts',(-0.342469011252512,0.698867316238289,
5.42949607339388));
#9109=CARTESIAN_POINT('Ctrl Pts',(-0.707447256311363,0.334638873927445,
5.46341601587375));
#9110=CARTESIAN_POINT('Ctrl Pts',(-0.765942731942805,-0.180685845273631,
5.49752276624412));
#9111=CARTESIAN_POINT('Ctrl Pts',(-0.488977975671522,-0.622493468082251,
5.53182729600019));
#9112=CARTESIAN_POINT('Ctrl Pts',(0.00623870066985125,-0.79639957834953,
5.56633555615365));
#9113=CARTESIAN_POINT('Ctrl Pts',(0.411979748797062,-0.65451285296037,5.59462344155862));
#9114=CARTESIAN_POINT('Ctrl Pts',(0.628431910779513,-0.420156210117234,
5.61658281146561));
#9115=CARTESIAN_POINT('Ctrl Pts',(0.759739764112401,-0.149292484888909,
5.63730747934422));
#9116=CARTESIAN_POINT('Ctrl Pts',(0.759837930575591,0.241447639232068,5.66332246132793));
#9117=CARTESIAN_POINT('Ctrl Pts',(0.516864570620339,0.598828714990839,5.6921027083035));
#9118=CARTESIAN_POINT('Ctrl Pts',(0.16754402090728,0.766642660816134,5.7183984452765));
#9119=CARTESIAN_POINT('Ctrl Pts',(-0.18243289406626,0.766996703299491,5.74216819224318));
#9120=CARTESIAN_POINT('Ctrl Pts',(-0.499344694617947,0.614409373974203,
5.7660436717059));
#9121=CARTESIAN_POINT('Ctrl Pts',(-0.719666388043044,0.338417073722969,
5.79002421526266));
#9122=CARTESIAN_POINT('Ctrl Pts',(-0.798838486989696,-0.00747184320142611,
5.81411179267834));
#9123=CARTESIAN_POINT('Ctrl Pts',(-0.732821087254027,-0.296979929993814,
5.83427424859502));
#9124=CARTESIAN_POINT('Ctrl Pts',(-0.608236501384017,-0.494969333219339,
5.85045910955365));
#9125=CARTESIAN_POINT('Ctrl Pts',(-0.442617486739659,-0.660891288693568,
5.8666802534398));
#9126=CARTESIAN_POINT('Ctrl Pts',(-0.172748327050428,-0.791093551297648,
5.88702427548063));
#9127=CARTESIAN_POINT('Ctrl Pts',(0.188434824933959,-0.791259517626132,
5.91154722254856));
#9128=CARTESIAN_POINT('Ctrl Pts',(0.515509148139609,-0.63399975107043,5.93618028019028));
#9129=CARTESIAN_POINT('Ctrl Pts',(0.742660619778638,-0.349226128508519,
5.96092404661359));
#9130=CARTESIAN_POINT('Ctrl Pts',(0.834013573979388,0.047387173011833,5.98854018010049));
#9131=CARTESIAN_POINT('Ctrl Pts',(0.699054298781812,0.485509196729349,6.01907630606175));
#9132=CARTESIAN_POINT('Ctrl Pts',(0.306089489608805,0.800037047528466,6.05258598067156));
#9133=CARTESIAN_POINT('Ctrl Pts',(-0.198806257075136,0.83811783046203,6.08629244673437));
#9134=CARTESIAN_POINT('Ctrl Pts',(-0.639994604888811,0.58386009688861,6.12019546148202));
#9135=CARTESIAN_POINT('Ctrl Pts',(-0.862778510831916,0.122809110352501,
6.15429381358228));
#9136=CARTESIAN_POINT('Ctrl Pts',(-0.783768475044449,-0.408002461396071,
6.19001514975991));
#9137=CARTESIAN_POINT('Ctrl Pts',(-0.382461984654271,-0.810530499122485,
6.22738726758261));
#9138=CARTESIAN_POINT('Ctrl Pts',(0.141571880318707,-0.869426431241229,
6.26209856247513));
#9139=CARTESIAN_POINT('Ctrl Pts',(0.546857792365987,-0.673923824775829,
6.29262411862805));
#9140=CARTESIAN_POINT('Ctrl Pts',(0.787850231799947,-0.371686474029746,
6.31889326617887));
#9141=CARTESIAN_POINT('Ctrl Pts',(0.889701212277186,0.0702541647771362,
6.34966096595927));
#9142=CARTESIAN_POINT('Ctrl Pts',(0.713512875154728,0.577124702757749,6.38499463961466));
#9143=CARTESIAN_POINT('Ctrl Pts',(0.198967909509621,0.901053551471294,6.42496855240101));
#9144=CARTESIAN_POINT('Ctrl Pts',(-0.408089575093021,0.833131022176632,
6.46516128973043));
#9145=CARTESIAN_POINT('Ctrl Pts',(-0.842862380754781,0.399211540997894,
6.50556671739343));
#9146=CARTESIAN_POINT('Ctrl Pts',(-0.912482057616401,-0.214227019813974,
6.54617863195434));
#9147=CARTESIAN_POINT('Ctrl Pts',(-0.582857572239619,-0.739804921207224,
6.58699019870486));
#9148=CARTESIAN_POINT('Ctrl Pts',(0.00529210032697009,-0.946120388887076,
6.62799422182894));
#9149=CARTESIAN_POINT('Ctrl Pts',(0.596417413889089,-0.73978975515068,6.66918308377763));
#9150=CARTESIAN_POINT('Ctrl Pts',(0.931157121946736,-0.20751322428765,6.71054882574604));
#9151=CARTESIAN_POINT('Ctrl Pts',(0.861650483779265,0.419727599707763,6.75208097200662));
#9152=CARTESIAN_POINT('Ctrl Pts',(0.413147604956643,0.868498049400113,6.79377525221771));
#9153=CARTESIAN_POINT('Ctrl Pts',(-0.148210983168275,0.931421962876526,
6.83097036528324));
#9154=CARTESIAN_POINT('Ctrl Pts',(-0.581294729795694,0.722118347875597,
6.86360544825447));
#9155=CARTESIAN_POINT('Ctrl Pts',(-0.838871906802363,0.399682199015836,
6.89163933377065));
#9156=CARTESIAN_POINT('Ctrl Pts',(-0.930877231252504,-0.00373870819751691,
6.91972773631357));
#9157=CARTESIAN_POINT('Ctrl Pts',(-0.838749751075799,-0.407817095097561,
6.94787183402895));
#9158=CARTESIAN_POINT('Ctrl Pts',(-0.579931993725618,-0.732521582072749,
6.9760659349542));
#9159=CARTESIAN_POINT('Ctrl Pts',(-0.205212822112969,-0.913124822787424,
7.00430873475179));
#9160=CARTESIAN_POINT('Ctrl Pts',(0.211338054228992,-0.913070414334495,
7.03259350527625));
#9161=CARTESIAN_POINT('Ctrl Pts',(0.587263134138024,-0.732110657981568,
7.06092123472863));
#9162=CARTESIAN_POINT('Ctrl Pts',(0.847742099102453,-0.405599817717801,
7.08928670598057));
#9163=CARTESIAN_POINT('Ctrl Pts',(0.940948978785284,0.00228770078596691,
7.1176867396323));
#9164=CARTESIAN_POINT('Ctrl Pts',(0.847659354457111,0.410238520315532,7.14611819660086));
#9165=CARTESIAN_POINT('Ctrl Pts',(0.543275903219406,0.793339172582683,7.17932027275837));
#9166=CARTESIAN_POINT('Ctrl Pts',(-0.001093578869141,0.984623315384901,
7.21730924712761));
#9167=CARTESIAN_POINT('Ctrl Pts',(-0.615252284949225,0.769726133995085,
7.26008973650359));
#9168=CARTESIAN_POINT('Ctrl Pts',(-0.961422256849412,0.218820343216691,
7.30290266259028));
#9169=CARTESIAN_POINT('Ctrl Pts',(-0.888633848724617,-0.428292780832149,
7.34573759998394));
#9170=CARTESIAN_POINT('Ctrl Pts',(-0.42811642962634,-0.888746898872104,
7.38857936211361));
#9171=CARTESIAN_POINT('Ctrl Pts',(0.218959376739582,-0.961833511797225,
7.43142516328682));
#9172=CARTESIAN_POINT('Ctrl Pts',(0.770122900311167,-0.615157339727794,
7.47424382285298));
#9173=CARTESIAN_POINT('Ctrl Pts',(0.913207865694905,-0.206388594750497,
7.5027957331042));
#9174=CARTESIAN_POINT('Ctrl Pts',(0.913235549072487,-0.00119827763899913,
7.51704057274925));
#9175=CARTESIAN_POINT('Ctrl Pts',(0.688502394196997,-0.00177585944161231,
5.42536374837757));
#9176=CARTESIAN_POINT('Ctrl Pts',(0.688481448875166,0.153471500858794,5.43614141945633));
#9177=CARTESIAN_POINT('Ctrl Pts',(0.580508040541705,0.46124670025465,5.45764245524231));
#9178=CARTESIAN_POINT('Ctrl Pts',(0.165662319023174,0.722161337503787,5.48987538957648));
#9179=CARTESIAN_POINT('Ctrl Pts',(-0.320578571387279,0.667050889553626,
5.52206618528612));
#9180=CARTESIAN_POINT('Ctrl Pts',(-0.666378826232044,0.32127882597957,5.55424091986707));
#9181=CARTESIAN_POINT('Ctrl Pts',(-0.721063694800031,-0.164642450695304,
5.58640440743116));
#9182=CARTESIAN_POINT('Ctrl Pts',(-0.461013415699651,-0.578597703078686,
5.61857188153771));
#9183=CARTESIAN_POINT('Ctrl Pts',(0.000868763121645957,-0.740322038056404,
5.65075229330461));
#9184=CARTESIAN_POINT('Ctrl Pts',(0.377087016267437,-0.608394442936668,
5.67699673395361));
#9185=CARTESIAN_POINT('Ctrl Pts',(0.577057627822796,-0.391810817241549,
5.69729012722977));
#9186=CARTESIAN_POINT('Ctrl Pts',(0.698092236754842,-0.142020837867168,
5.71640197572506));
#9187=CARTESIAN_POINT('Ctrl Pts',(0.697963439505406,0.21710900600399,5.74031529151263));
#9188=CARTESIAN_POINT('Ctrl Pts',(0.475355133020151,0.544099194249106,5.76666169992576));
#9189=CARTESIAN_POINT('Ctrl Pts',(0.156654851678278,0.697080460332168,5.79065302227195));
#9190=CARTESIAN_POINT('Ctrl Pts',(-0.161711917448867,0.697304453295988,
5.81227877536069));
#9191=CARTESIAN_POINT('Ctrl Pts',(-0.449161842092396,0.558802207686871,
5.83393922469739));
#9192=CARTESIAN_POINT('Ctrl Pts',(-0.648454473279016,0.309008113535057,
5.85564132087709));
#9193=CARTESIAN_POINT('Ctrl Pts',(-0.719837707005216,-0.00322310267600228,
5.8773860839056));
#9194=CARTESIAN_POINT('Ctrl Pts',(-0.660324209075774,-0.263926195140504,
5.89554604949557));
#9195=CARTESIAN_POINT('Ctrl Pts',(-0.548312630732919,-0.441913047209008,
5.91009721234879));
#9196=CARTESIAN_POINT('Ctrl Pts',(-0.399568209162923,-0.590912445741052,
5.92466534563453));
#9197=CARTESIAN_POINT('Ctrl Pts',(-0.157550820881924,-0.70761172499092,
5.94291010238594));
#9198=CARTESIAN_POINT('Ctrl Pts',(0.165683821816319,-0.707692893763189,
5.96485832442363));
#9199=CARTESIAN_POINT('Ctrl Pts',(0.457834734757014,-0.567156151977817,
5.98686542599537));
#9200=CARTESIAN_POINT('Ctrl Pts',(0.660365135739603,-0.313163685177989,
6.00893343132688));
#9201=CARTESIAN_POINT('Ctrl Pts',(0.741647053339758,0.0400023925443897,
6.03352542353788));
#9202=CARTESIAN_POINT('Ctrl Pts',(0.6215856897095,0.429424608756888,6.0606712019436));
#9203=CARTESIAN_POINT('Ctrl Pts',(0.272788863259715,0.708464025234,6.09040985442785));
#9204=CARTESIAN_POINT('Ctrl Pts',(-0.174640201386968,0.742128787355836,
6.12028246378202));
#9205=CARTESIAN_POINT('Ctrl Pts',(-0.565102038705666,0.517026489502915,
6.1502917775661));
#9206=CARTESIAN_POINT('Ctrl Pts',(-0.762043624567604,0.109327312662896,
6.18044350600909));
#9207=CARTESIAN_POINT('Ctrl Pts',(-0.692189456122551,-0.359678326088431,
6.21200701480215));
#9208=CARTESIAN_POINT('Ctrl Pts',(-0.337773460931687,-0.715129603852559,
6.24501197076816));
#9209=CARTESIAN_POINT('Ctrl Pts',(0.124866016940657,-0.767119798247897,
6.27565761479799));
#9210=CARTESIAN_POINT('Ctrl Pts',(0.482663833907203,-0.594530247737682,
6.30260654020584));
#9211=CARTESIAN_POINT('Ctrl Pts',(0.695450511759543,-0.32768100442103,6.32580056862507));
#9212=CARTESIAN_POINT('Ctrl Pts',(0.785412896461935,0.0626075158038052,
6.35297268106789));
#9213=CARTESIAN_POINT('Ctrl Pts',(0.629799785153589,0.510459438093438,6.38419099540486));
#9214=CARTESIAN_POINT('Ctrl Pts',(0.174872432500897,0.796962684150136,6.41953687685404));
#9215=CARTESIAN_POINT('Ctrl Pts',(-0.362484676752387,0.736952725256016,
6.4551134881321));
#9216=CARTESIAN_POINT('Ctrl Pts',(-0.74792746534711,0.35245915978463,6.49092474388711));
#9217=CARTESIAN_POINT('Ctrl Pts',(-0.809887309570728,-0.192065947901566,
6.52697449126839));
#9218=CARTESIAN_POINT('Ctrl Pts',(-0.516915158076634,-0.65954619222211,
6.56326583721123));
#9219=CARTESIAN_POINT('Ctrl Pts',(0.00709632936792426,-0.843579839117015,
6.59980147205316));
#9220=CARTESIAN_POINT('Ctrl Pts',(0.535080054211952,-0.659528972736876,
6.63658345012356));
#9221=CARTESIAN_POINT('Ctrl Pts',(0.834961098454938,-0.183143056575008,
6.67361341976074));
#9222=CARTESIAN_POINT('Ctrl Pts',(0.772836475154942,0.379911298835229,6.71089252375131));
#9223=CARTESIAN_POINT('Ctrl Pts',(0.369319867823668,0.784090370590367,6.74842072124706));
#9224=CARTESIAN_POINT('Ctrl Pts',(-0.137507651352654,0.841177037621035,
6.78200064499767));
#9225=CARTESIAN_POINT('Ctrl Pts',(-0.529655686323561,0.651783755111279,
6.81154496618753));
#9226=CARTESIAN_POINT('Ctrl Pts',(-0.763440172149879,0.359289385813127,
6.83697845361481));
#9227=CARTESIAN_POINT('Ctrl Pts',(-0.847211586055085,-0.0075813723717918,
6.86252259094478));
#9228=CARTESIAN_POINT('Ctrl Pts',(-0.763337400290734,-0.37595112739322,
6.88817526440515));
#9229=CARTESIAN_POINT('Ctrl Pts',(-0.526914388323573,-0.672730225787424,
6.91393691075106));
#9230=CARTESIAN_POINT('Ctrl Pts',(-0.183698562689997,-0.838276618909781,
6.93980597887144));
#9231=CARTESIAN_POINT('Ctrl Pts',(0.198889088741007,-0.838335964394735,
6.96578323697683));
#9232=CARTESIAN_POINT('Ctrl Pts',(0.545106947003364,-0.67180754918665,6.99186582148597));
#9233=CARTESIAN_POINT('Ctrl Pts',(0.785703595073577,-0.370406649743822,
7.01805361583897));
#9234=CARTESIAN_POINT('Ctrl Pts',(0.872119316826772,0.00721196141493378,
7.04434542939925));
#9235=CARTESIAN_POINT('Ctrl Pts',(0.785618184490446,0.386004597261683,7.07073989965295));
#9236=CARTESIAN_POINT('Ctrl Pts',(0.502331801959327,0.742799085163601,7.10165209474801));
#9237=CARTESIAN_POINT('Ctrl Pts',(-0.00621863503242753,0.921910367253639,
7.13714527690347));
#9238=CARTESIAN_POINT('Ctrl Pts',(-0.582851103775203,0.720649175322028,
7.17729562502998));
#9239=CARTESIAN_POINT('Ctrl Pts',(-0.909668842554882,0.201440782148561,
7.21765904401918));
#9240=CARTESIAN_POINT('Ctrl Pts',(-0.841213659251149,-0.41162272843365,
7.25823121418976));
#9241=CARTESIAN_POINT('Ctrl Pts',(-0.403262459624705,-0.850227454077078,
7.29900198947476));
#9242=CARTESIAN_POINT('Ctrl Pts',(0.215483513378321,-0.920627886099326,
7.33997190269741));
#9243=CARTESIAN_POINT('Ctrl Pts',(0.745429336505933,-0.587899220267355,
7.3811170115228));
#9244=CARTESIAN_POINT('Ctrl Pts',(0.883871797949062,-0.193227595737394,
7.40868621059601));
#9245=CARTESIAN_POINT('Ctrl Pts',(0.8838985919702,0.0053707753556189,7.42247342039135));
#9246=CARTESIAN_POINT('Ctrl Pts',(0.750293052325257,-0.00715957249020984,
5.50303372536175));
#9247=CARTESIAN_POINT('Ctrl Pts',(0.750270265731315,0.161735352510056,5.51475884548619));
#9248=CARTESIAN_POINT('Ctrl Pts',(0.632695708259348,0.496355890433882,5.53813632129441));
#9249=CARTESIAN_POINT('Ctrl Pts',(0.18381648383294,0.778081359279531,5.57298649818651));
#9250=CARTESIAN_POINT('Ctrl Pts',(-0.339280552431234,0.718378415257623,
5.6076202896276));
#9251=CARTESIAN_POINT('Ctrl Pts',(-0.709001801655557,0.347985187059841,
5.64204689091912));
#9252=CARTESIAN_POINT('Ctrl Pts',(-0.766698885918436,-0.16919180614749,
5.67627188750895));
#9253=CARTESIAN_POINT('Ctrl Pts',(-0.491102255096102,-0.606944769908898,
5.71030250431352));
#9254=CARTESIAN_POINT('Ctrl Pts',(-0.00508600093609879,-0.776552326514125,
5.74414714312887));
#9255=CARTESIAN_POINT('Ctrl Pts',(0.388081485630343,-0.638236893263609,
5.77157703947433));
#9256=CARTESIAN_POINT('Ctrl Pts',(0.596158844376195,-0.412773207290159,
5.79269814069561));
#9257=CARTESIAN_POINT('Ctrl Pts',(0.721744080724043,-0.15346691557969,5.81253217830301));
#9258=CARTESIAN_POINT('Ctrl Pts',(0.721291797138653,0.217701679185308,5.83724463136508));
#9259=CARTESIAN_POINT('Ctrl Pts',(0.492248297398938,0.553560023202817,5.86431639993153));
#9260=CARTESIAN_POINT('Ctrl Pts',(0.166319730891556,0.709798906698298,5.88884215604732));
#9261=CARTESIAN_POINT('Ctrl Pts',(-0.157783238149665,0.709878237357754,
5.9108529793775));
#9262=CARTESIAN_POINT('Ctrl Pts',(-0.449076273551193,0.569337590676698,
5.9328067996584));
#9263=CARTESIAN_POINT('Ctrl Pts',(-0.650064161571041,0.317172677340155,
5.95470251296732));
#9264=CARTESIAN_POINT('Ctrl Pts',(-0.721621885005776,0.00344024431033504,
5.97654562679051));
#9265=CARTESIAN_POINT('Ctrl Pts',(-0.661964542748072,-0.257286466758943,
5.99470556888389));
#9266=CARTESIAN_POINT('Ctrl Pts',(-0.550269179200512,-0.434720760832016,
6.00921182085571));
#9267=CARTESIAN_POINT('Ctrl Pts',(-0.402276742496014,-0.58292974874922,
6.02370295744568));
#9268=CARTESIAN_POINT('Ctrl Pts',(-0.162278225783224,-0.698511519651894,
6.04178723904388));
#9269=CARTESIAN_POINT('Ctrl Pts',(0.15678598762643,-0.698434753182134,6.06344900909546));
#9270=CARTESIAN_POINT('Ctrl Pts',(0.443832361536606,-0.560174670954122,
6.0850728430943));
#9271=CARTESIAN_POINT('Ctrl Pts',(0.641886657484862,-0.311548705127534,
6.10666325451466));
#9272=CARTESIAN_POINT('Ctrl Pts',(0.720903708581916,0.0325797868375459,
6.13061738623125));
#9273=CARTESIAN_POINT('Ctrl Pts',(0.604189885592221,0.409985700434759,6.15692940855218));
#9274=CARTESIAN_POINT('Ctrl Pts',(0.267732283871283,0.678698793729311,6.1855932204343));
#9275=CARTESIAN_POINT('Ctrl Pts',(-0.161176377088454,0.710602415331958,
6.2142207026778));
#9276=CARTESIAN_POINT('Ctrl Pts',(-0.53324499976805,0.49569736156826,6.2428252689349));
#9277=CARTESIAN_POINT('Ctrl Pts',(-0.71970802918005,0.108916638193807,6.27141553040571));
#9278=CARTESIAN_POINT('Ctrl Pts',(-0.653459538269235,-0.333490314335375,
6.30118792123758));
#9279=CARTESIAN_POINT('Ctrl Pts',(-0.320608653043408,-0.666665722932101,
6.33214798295712));
#9280=CARTESIAN_POINT('Ctrl Pts',(0.11110066391128,-0.714779997862643,6.36073732994674));
#9281=CARTESIAN_POINT('Ctrl Pts',(0.443426222920022,-0.554309028733026,
6.38577168766062));
#9282=CARTESIAN_POINT('Ctrl Pts',(0.640332263629123,-0.307185736963075,
6.4072429033775));
#9283=CARTESIAN_POINT('Ctrl Pts',(0.723203970884255,0.0529817392810816,
6.43231277693535));
#9284=CARTESIAN_POINT('Ctrl Pts',(0.579875213873492,0.464421357446747,6.46099511352603));
#9285=CARTESIAN_POINT('Ctrl Pts',(0.163540281833546,0.726164737539782,6.49332268601409));
#9286=CARTESIAN_POINT('Ctrl Pts',(-0.325806422280217,0.671154653749907,
6.52571901232898));
#9287=CARTESIAN_POINT('Ctrl Pts',(-0.675167952131389,0.322177709778464,
6.55819617950246));
#9288=CARTESIAN_POINT('Ctrl Pts',(-0.730838200739421,-0.169856078141101,
6.59076464701581));
#9289=CARTESIAN_POINT('Ctrl Pts',(-0.466820433339978,-0.590588090246883,
6.62343536526493));
#9290=CARTESIAN_POINT('Ctrl Pts',(0.00350996735505748,-0.755486408003205,
6.65621873257887));
#9291=CARTESIAN_POINT('Ctrl Pts',(0.475826092423244,-0.590582675084604,
6.6891250935537));
#9292=CARTESIAN_POINT('Ctrl Pts',(0.743223728972327,-0.165383236018042,
6.72216417731904));
#9293=CARTESIAN_POINT('Ctrl Pts',(0.687732640812107,0.335833673405217,6.75534872287688));
#9294=CARTESIAN_POINT('Ctrl Pts',(0.329161852114402,0.69473766380513,6.78868194987952));
#9295=CARTESIAN_POINT('Ctrl Pts',(-0.120255207878517,0.745235334942848,
6.81845529502086));
#9296=CARTESIAN_POINT('Ctrl Pts',(-0.467524502978826,0.57746640430216,6.84461903462784));
#9297=CARTESIAN_POINT('Ctrl Pts',(-0.674360922287096,0.318638588168112,
6.86712201294724));
#9298=CARTESIAN_POINT('Ctrl Pts',(-0.748404023106268,-0.00575219575844088,
6.88970750051041));
#9299=CARTESIAN_POINT('Ctrl Pts',(-0.674269101945005,-0.331252076513231,
6.91237414913092));
#9300=CARTESIAN_POINT('Ctrl Pts',(-0.465442485762675,-0.593360030871918,
6.93512642552479));
#9301=CARTESIAN_POINT('Ctrl Pts',(-0.162413298418938,-0.73950734230565,
6.95796516185281));
#9302=CARTESIAN_POINT('Ctrl Pts',(0.175299902719076,-0.739551441572441,
6.98089514210305));
#9303=CARTESIAN_POINT('Ctrl Pts',(0.48087309657339,-0.592568368954699,7.00391530912488));
#9304=CARTESIAN_POINT('Ctrl Pts',(0.693231099227059,-0.326542805878524,
7.02702898588934));
#9305=CARTESIAN_POINT('Ctrl Pts',(0.769520632376555,0.00680181224901938,
7.05023795575404));
#9306=CARTESIAN_POINT('Ctrl Pts',(0.693149586424791,0.341276467608696,7.07354385445611));
#9307=CARTESIAN_POINT('Ctrl Pts',(0.442928349106893,0.656453792431941,7.1008495131406));
#9308=CARTESIAN_POINT('Ctrl Pts',(-0.00655006027916784,0.814828143116751,
7.13222145322597));
#9309=CARTESIAN_POINT('Ctrl Pts',(-0.51677651805262,0.636849892039306,7.16774598353412));
#9310=CARTESIAN_POINT('Ctrl Pts',(-0.806409087124653,0.176948274600164,
7.20350474142154));
#9311=CARTESIAN_POINT('Ctrl Pts',(-0.745817965655065,-0.367012141382838,
7.2395023580954));
#9312=CARTESIAN_POINT('Ctrl Pts',(-0.356682875026977,-0.756951656680894,
7.27574101303561));
#9313=CARTESIAN_POINT('Ctrl Pts',(0.194324484528691,-0.819874060139303,
7.3122257656988));
#9314=CARTESIAN_POINT('Ctrl Pts',(0.667449116817723,-0.523027248491166,
7.34895409901446));
#9315=CARTESIAN_POINT('Ctrl Pts',(0.791458463792618,-0.170101188152833,
7.37361186684348));
#9316=CARTESIAN_POINT('Ctrl Pts',(0.791482481276893,0.00791737913227817,
7.38597037371902));
#9317=CARTESIAN_POINT('Ctrl Pts',(0.849598076317196,-0.00712734349710777,
5.50276247098815));
#9318=CARTESIAN_POINT('Ctrl Pts',(0.849572315215897,0.183814720194332,5.51601816019011));
#9319=CARTESIAN_POINT('Ctrl Pts',(0.716484451910036,0.562864504493882,5.5424997573337));
#9320=CARTESIAN_POINT('Ctrl Pts',(0.20809212706776,0.881898014322701,5.58196713633214));
#9321=CARTESIAN_POINT('Ctrl Pts',(-0.384533142466098,0.814321092392168,
5.6212091202806));
#9322=CARTESIAN_POINT('Ctrl Pts',(-0.803342488001547,0.394693505033448,
5.66020880663821));
#9323=CARTESIAN_POINT('Ctrl Pts',(-0.868627634713463,-0.190973266163329,
5.69896909964657));
#9324=CARTESIAN_POINT('Ctrl Pts',(-0.556653040774226,-0.686349150395686,
5.7374846668518));
#9325=CARTESIAN_POINT('Ctrl Pts',(-0.00707997145394115,-0.878014145711534,
5.77575459287924));
#9326=CARTESIAN_POINT('Ctrl Pts',(0.436900544149483,-0.72169954588876,5.80673549990624));
#9327=CARTESIAN_POINT('Ctrl Pts',(0.671606542222444,-0.467350263792894,
5.83056225412086));
#9328=CARTESIAN_POINT('Ctrl Pts',(0.813155385970533,-0.1750292179711,5.85292188205288));
#9329=CARTESIAN_POINT('Ctrl Pts',(0.812540057938428,0.242883178054026,5.88074814557167));
#9330=CARTESIAN_POINT('Ctrl Pts',(0.554998700939117,0.6202772367454,5.91117655608676));
#9331=CARTESIAN_POINT('Ctrl Pts',(0.189304493774159,0.795493011487289,5.93869516979536));
#9332=CARTESIAN_POINT('Ctrl Pts',(-0.173712239990491,0.795504865118224,
5.96335163063203));
#9333=CARTESIAN_POINT('Ctrl Pts',(-0.499345414071431,0.638313353697133,
5.98789731654311));
#9334=CARTESIAN_POINT('Ctrl Pts',(-0.72356068389146,0.356867037202337,6.01233388291633));
#9335=CARTESIAN_POINT('Ctrl Pts',(-0.803163168357719,0.00747357176146625,
6.03666105392709));
#9336=CARTESIAN_POINT('Ctrl Pts',(-0.736797982336716,-0.28222992698738,
6.05684360012597));
#9337=CARTESIAN_POINT('Ctrl Pts',(-0.612891815719577,-0.479031268493863,
6.07293511022899));
#9338=CARTESIAN_POINT('Ctrl Pts',(-0.448917230819194,-0.643222296978376,
6.08899082487842));
#9339=CARTESIAN_POINT('Ctrl Pts',(-0.18345184155449,-0.770972157981274,
6.10899459772628));
#9340=CARTESIAN_POINT('Ctrl Pts',(0.168509519247147,-0.770779631725406,
6.1328926650123));
#9341=CARTESIAN_POINT('Ctrl Pts',(0.484258307101598,-0.618569501699951,
6.15668614964677));
#9342=CARTESIAN_POINT('Ctrl Pts',(0.7014559478794,-0.345739709198507,6.18037560572192));
#9343=CARTESIAN_POINT('Ctrl Pts',(0.787759201210554,0.0307483449030446,
6.20658402952268));
#9344=CARTESIAN_POINT('Ctrl Pts',(0.660297100374137,0.44205148705441,6.23526827245269));
#9345=CARTESIAN_POINT('Ctrl Pts',(0.29489586174265,0.733477282971818,6.2663838499292));
#9346=CARTESIAN_POINT('Ctrl Pts',(-0.168647261234911,0.767641847640704,
6.2973293246475));
#9347=CARTESIAN_POINT('Ctrl Pts',(-0.568727882191308,0.536181820843462,
6.32810567535681));
#9348=CARTESIAN_POINT('Ctrl Pts',(-0.768048251626985,0.121961889290114,
6.35871685457357));
#9349=CARTESIAN_POINT('Ctrl Pts',(-0.697107833504566,-0.349296397819721,
6.39043824166099));
#9350=CARTESIAN_POINT('Ctrl Pts',(-0.344045555812211,-0.701995892428354,
6.42325363059534));
#9351=CARTESIAN_POINT('Ctrl Pts',(0.110773521189623,-0.752235352072163,
6.45337778122228));
#9352=CARTESIAN_POINT('Ctrl Pts',(0.458965638454581,-0.583886825258837,
6.47961716649731));
#9353=CARTESIAN_POINT('Ctrl Pts',(0.664381883487217,-0.325864755846388,
6.50203114286227));
#9354=CARTESIAN_POINT('Ctrl Pts',(0.750332653299937,0.0485776788759206,
6.52809351690923));
#9355=CARTESIAN_POINT('Ctrl Pts',(0.601674226486008,0.473897649396157,6.55776163974272));
#9356=CARTESIAN_POINT('Ctrl Pts',(0.173613673117217,0.742348086642931,6.59098287751551));
#9357=CARTESIAN_POINT('Ctrl Pts',(-0.3258350440189,0.685649541287933,6.62406030334558));
#9358=CARTESIAN_POINT('Ctrl Pts',(-0.679731238547397,0.331354382468774,
6.65700275666622));
#9359=CARTESIAN_POINT('Ctrl Pts',(-0.735255898447251,-0.164397347346024,
6.6898206739066));
#9360=CARTESIAN_POINT('Ctrl Pts',(-0.470558029977308,-0.585159244984441,
6.7225241569716));
#9361=CARTESIAN_POINT('Ctrl Pts',(-0.00278192751448173,-0.748569972495831,
6.75512382817215));
#9362=CARTESIAN_POINT('Ctrl Pts',(0.46350519113553,-0.58518407843876,6.78763042208935));
#9363=CARTESIAN_POINT('Ctrl Pts',(0.725410474458316,-0.167706567477984,
6.82005514647598));
#9364=CARTESIAN_POINT('Ctrl Pts',(0.670774587918448,0.320804047707368,6.85240545447397));
#9365=CARTESIAN_POINT('Ctrl Pts',(0.323092957157568,0.668041717311718,6.88470045447928));
#9366=CARTESIAN_POINT('Ctrl Pts',(-0.109494451463983,0.716184576245998,
6.91336373465137));
#9367=CARTESIAN_POINT('Ctrl Pts',(-0.44188826662967,0.555407233522295,6.93841735921765));
#9368=CARTESIAN_POINT('Ctrl Pts',(-0.639012403336459,0.308500858246645,
6.95988071793453));
#9369=CARTESIAN_POINT('Ctrl Pts',(-0.709192507424316,0.00040641570270789,
6.98133136104379));
#9370=CARTESIAN_POINT('Ctrl Pts',(-0.638918625948615,-0.307487189319304,
7.00277862675193));
#9371=CARTESIAN_POINT('Ctrl Pts',(-0.442028652642433,-0.554399048208452,
7.02422233485342));
#9372=CARTESIAN_POINT('Ctrl Pts',(-0.157482946544586,-0.691481626684627,
7.0456683320825));
#9373=CARTESIAN_POINT('Ctrl Pts',(0.15835851542768,-0.691398914091788,7.06711532573104));
#9374=CARTESIAN_POINT('Ctrl Pts',(0.44307547960184,-0.554307235545146,7.08857226527194));
#9375=CARTESIAN_POINT('Ctrl Pts',(0.64018584092255,-0.307192493791569,7.11004002498397));
#9376=CARTESIAN_POINT('Ctrl Pts',(0.71067332605218,0.00132671397574847,
7.13152214083118));
#9377=CARTESIAN_POINT('Ctrl Pts',(0.640127181409651,0.309809306958141,7.15302225181439));
#9378=CARTESIAN_POINT('Ctrl Pts',(0.409965562319378,0.59950154513597,7.1781297331652));
#9379=CARTESIAN_POINT('Ctrl Pts',(-0.00180430761257666,0.744250295435473,
7.20686838534354));
#9380=CARTESIAN_POINT('Ctrl Pts',(-0.46689999412445,0.581628177637233,7.23926440850474));
#9381=CARTESIAN_POINT('Ctrl Pts',(-0.729602505011613,0.163869023223047,
7.27173917712393));
#9382=CARTESIAN_POINT('Ctrl Pts',(-0.674485616164893,-0.328104186907804,
7.3043020520652));
#9383=CARTESIAN_POINT('Ctrl Pts',(-0.32358572160231,-0.679299557613987,
7.33696613118188));
#9384=CARTESIAN_POINT('Ctrl Pts',(0.171370920939519,-0.735610678055291,
7.36973771478191));
#9385=CARTESIAN_POINT('Ctrl Pts',(0.594929256360531,-0.469509634858928,
7.40263639340595));
#9386=CARTESIAN_POINT('Ctrl Pts',(0.705563583847616,-0.154509464242322,
7.42464584593578));
#9387=CARTESIAN_POINT('Ctrl Pts',(0.705585033709163,0.00447777927316105,
7.4356831493591));
#9388=CARTESIAN_POINT('Ctrl Pts',(0.911787311372316,-0.00175313599507732,
5.42547035947661));
#9389=CARTESIAN_POINT('Ctrl Pts',(0.911759679946333,0.203051830949188,5.43968844708048));
#9390=CARTESIAN_POINT('Ctrl Pts',(0.768907437119982,0.61071591344494,5.46816718430648));
#9391=CARTESIAN_POINT('Ctrl Pts',(0.220284165601068,0.955502366817236,5.51077805671262));
#9392=CARTESIAN_POINT('Ctrl Pts',(-0.422243656323184,0.882710139668278,
5.55332558349325));
#9393=CARTESIAN_POINT('Ctrl Pts',(-0.878386039542625,0.426289581625414,
5.5957765844892));
#9394=CARTESIAN_POINT('Ctrl Pts',(-0.950141006447777,-0.213553723589873,
5.63813025439539));
#9395=CARTESIAN_POINT('Ctrl Pts',(-0.60835728725253,-0.757014115469509,
5.68037224924266));
#9396=CARTESIAN_POINT('Ctrl Pts',(-0.00366338310403281,-0.968314430281517,
5.72249300107482));
#9397=CARTESIAN_POINT('Ctrl Pts',(0.486718248881734,-0.795970516833383,
5.75670865791863));
#9398=CARTESIAN_POINT('Ctrl Pts',(0.74653021351722,-0.514477549037207,5.78308078863264));
#9399=CARTESIAN_POINT('Ctrl Pts',(0.903446118847398,-0.190511009717507,
5.80786424281498));
#9400=CARTESIAN_POINT('Ctrl Pts',(0.90295145376886,0.273634535370419,5.8387700025228));
#9401=CARTESIAN_POINT('Ctrl Pts',(0.616343546706946,0.693954207986666,5.87265196790731));
#9402=CARTESIAN_POINT('Ctrl Pts',(0.208328450290096,0.889559871552857,5.90335942490417));
#9403=CARTESIAN_POINT('Ctrl Pts',(-0.197431208021256,0.889652469467467,
5.93091996947637));
#9404=CARTESIAN_POINT('Ctrl Pts',(-0.562029250439909,0.713737268348937,
5.95840063131195));
#9405=CARTESIAN_POINT('Ctrl Pts',(-0.813494233574056,0.39820149627948,5.98580131723829));
#9406=CARTESIAN_POINT('Ctrl Pts',(-0.902946074851847,0.0058870464447316,
6.01311843029465));
#9407=CARTESIAN_POINT('Ctrl Pts',(-0.828377509677636,-0.319866751453087,
6.03581174060078));
#9408=CARTESIAN_POINT('Ctrl Pts',(-0.688936970150508,-0.541360820821501,
6.05392170180393));
#9409=CARTESIAN_POINT('Ctrl Pts',(-0.504293132651573,-0.726263454623667,
6.07200206864918));
#9410=CARTESIAN_POINT('Ctrl Pts',(-0.205118119105362,-0.870286210128437,
6.0945471479209));
#9411=CARTESIAN_POINT('Ctrl Pts',(0.191971983732839,-0.870117700265186,
6.12150897978661));
#9412=CARTESIAN_POINT('Ctrl Pts',(0.548553466642107,-0.698273117288175,
6.14837718076188));
#9413=CARTESIAN_POINT('Ctrl Pts',(0.794052616995502,-0.389950825708538,
6.17514969693223));
#9414=CARTESIAN_POINT('Ctrl Pts',(0.891698024550524,0.0358312226908213,
6.20478886300642));
#9415=CARTESIAN_POINT('Ctrl Pts',(0.74749095040922,0.501334011480795,6.23725086378811));
#9416=CARTESIAN_POINT('Ctrl Pts',(0.333743343393983,0.831378563455359,6.27248425191807));
#9417=CARTESIAN_POINT('Ctrl Pts',(-0.19134387466354,0.870105625426578,6.3075348767601));
#9418=CARTESIAN_POINT('Ctrl Pts',(-0.644616547373273,0.607881105022717,
6.34239973374175));
#9419=CARTESIAN_POINT('Ctrl Pts',(-0.870417110421222,0.138612855199806,
6.37707657725051));
#9420=CARTESIAN_POINT('Ctrl Pts',(-0.790048775469081,-0.39510788351932,
6.41299953612703));
#9421=CARTESIAN_POINT('Ctrl Pts',(-0.390383204661376,-0.794274173322802,
6.45013660062964));
#9422=CARTESIAN_POINT('Ctrl Pts',(0.123964069137483,-0.851002982786416,
6.48419818277685));
#9423=CARTESIAN_POINT('Ctrl Pts',(0.517349958215306,-0.660759929294058,
6.51384272570464));
#9424=CARTESIAN_POINT('Ctrl Pts',(0.749191592206741,-0.369479150376496,
6.53914157276564));
#9425=CARTESIAN_POINT('Ctrl Pts',(0.846067098454331,0.052769037404062,6.56852738290555));
#9426=CARTESIAN_POINT('Ctrl Pts',(0.678541487051601,0.531594017531224,6.60192411587722));
#9427=CARTESIAN_POINT('Ctrl Pts',(0.197445708687755,0.833056774682923,6.63924640568331));
#9428=CARTESIAN_POINT('Ctrl Pts',(-0.362407034535075,0.76926077023711,6.67631865996902));
#9429=CARTESIAN_POINT('Ctrl Pts',(-0.757891257853047,0.372960662447378,
6.7131423125874));
#9430=CARTESIAN_POINT('Ctrl Pts',(-0.819502812158925,-0.17971389368945,
6.74971854734871));
#9431=CARTESIAN_POINT('Ctrl Pts',(-0.525117958852971,-0.647082052916212,
6.78604945080241));
#9432=CARTESIAN_POINT('Ctrl Pts',(-0.00706009915885147,-0.827706145589558,
6.82213749402266));
#9433=CARTESIAN_POINT('Ctrl Pts',(0.507168732938518,-0.647142083318005,
6.85798569667506));
#9434=CARTESIAN_POINT('Ctrl Pts',(0.794559460318739,-0.188312585352296,
6.89359746949419));
#9435=CARTESIAN_POINT('Ctrl Pts',(0.734412407851191,0.346047384757273,6.92898046138837));
#9436=CARTESIAN_POINT('Ctrl Pts',(0.35554627917015,0.723799648271606,6.96413145325235));
#9437=CARTESIAN_POINT('Ctrl Pts',(-0.113206435891536,0.775602232806529,
6.99517934888198));
#9438=CARTESIAN_POINT('Ctrl Pts',(-0.471799040782441,0.601968214167806,
7.0222090326148));
#9439=CARTESIAN_POINT('Ctrl Pts',(-0.6836661147338,0.336404243341276,7.04528069450069));
#9440=CARTESIAN_POINT('Ctrl Pts',(-0.758726003996092,0.0062400461075705,
7.06826344122686));
#9441=CARTESIAN_POINT('Ctrl Pts',(-0.6835849590214,-0.322409867084328,7.09115224380289));
#9442=CARTESIAN_POINT('Ctrl Pts',(-0.474072442185209,-0.584919976115439,
7.11395355010067));
#9443=CARTESIAN_POINT('Ctrl Pts',(-0.172560181698569,-0.730020088066619,
7.13666650878931));
#9444=CARTESIAN_POINT('Ctrl Pts',(0.16078217307758,-0.729778328929261,7.15929927954856));
#9445=CARTESIAN_POINT('Ctrl Pts',(0.459989212508115,-0.585545816121325,
7.18184723354721));
#9446=CARTESIAN_POINT('Ctrl Pts',(0.666223161118391,-0.32674631555655,7.20431603435277));
#9447=CARTESIAN_POINT('Ctrl Pts',(0.739554158501798,-0.00504686561265504,
7.22670799379599));
#9448=CARTESIAN_POINT('Ctrl Pts',(0.666159558065311,0.315205418031567,7.24902537021377));
#9449=CARTESIAN_POINT('Ctrl Pts',(0.428020561210259,0.614621005636118,7.27497954766194));
#9450=CARTESIAN_POINT('Ctrl Pts',(0.00440289337514439,0.763018006049135,
7.30452179484735));
#9451=CARTESIAN_POINT('Ctrl Pts',(-0.470624128322024,0.596319364034835,
7.33761244678054));
#9452=CARTESIAN_POINT('Ctrl Pts',(-0.736811683564632,0.171965979607826,
7.37056624676418));
#9453=CARTESIAN_POINT('Ctrl Pts',(-0.68068387352667,-0.324086643305756,
7.4033919913947));
#9454=CARTESIAN_POINT('Ctrl Pts',(-0.328791217341046,-0.675487864461335,
7.43610391008164));
#9455=CARTESIAN_POINT('Ctrl Pts',(0.163774412047771,-0.731012482418632,
7.4687018632077));
#9456=CARTESIAN_POINT('Ctrl Pts',(0.582152961317522,-0.467440680790944,
7.50121977146286));
#9457=CARTESIAN_POINT('Ctrl Pts',(0.690380552641563,-0.158133439986746,
7.52281364669809));
#9458=CARTESIAN_POINT('Ctrl Pts',(0.690401574315868,-0.00231993767140268,
7.53363062084317));
#9459=CARTESIAN_POINT('Ctrl Pts',(0.889359432826132,0.00495444760725769,
5.32880713791624));
#9460=CARTESIAN_POINT('Ctrl Pts',(0.889332447864276,0.204967802847453,5.34269257951066));
#9461=CARTESIAN_POINT('Ctrl Pts',(0.750004347575518,0.603672713614473,5.37053043303203));
#9462=CARTESIAN_POINT('Ctrl Pts',(0.21096706922133,0.94314460394843,5.41241969183905));
#9463=CARTESIAN_POINT('Ctrl Pts',(-0.423963274156834,0.87171349864309,5.45445132266662));
#9464=CARTESIAN_POINT('Ctrl Pts',(-0.877374490363263,0.418799407840054,
5.4966071161887));
#9465=CARTESIAN_POINT('Ctrl Pts',(-0.949545774103564,-0.219892556824646,
5.53888079270843));
#9466=CARTESIAN_POINT('Ctrl Pts',(-0.607068575689537,-0.765494054358749,
5.58125986451715));
#9467=CARTESIAN_POINT('Ctrl Pts',(0.00261167844658479,-0.97913119777945,
5.62373519298684));
#9468=CARTESIAN_POINT('Ctrl Pts',(0.499852533620251,-0.8048463257254,5.65841239967706));
#9469=CARTESIAN_POINT('Ctrl Pts',(0.764265215589788,-0.518466038803169,
5.68524380080038));
#9470=CARTESIAN_POINT('Ctrl Pts',(0.924328881255501,-0.188150671604858,
5.71051448038525));
#9471=CARTESIAN_POINT('Ctrl Pts',(0.924132430512447,0.286757902074732,5.74213409224145));
#9472=CARTESIAN_POINT('Ctrl Pts',(0.62986087869606,0.718937325916808,5.77695468815655));
#9473=CARTESIAN_POINT('Ctrl Pts',(0.208953775300158,0.920912997464213,5.80863418802737));
#9474=CARTESIAN_POINT('Ctrl Pts',(-0.211068988110463,0.921157282542793,
5.83716174516452));
#9475=CARTESIAN_POINT('Ctrl Pts',(-0.589810577699277,0.738585626106938,
5.86570218738055));
#9476=CARTESIAN_POINT('Ctrl Pts',(-0.85194552766839,0.409898301969846,5.89425134138179));
#9477=CARTESIAN_POINT('Ctrl Pts',(-0.945597945878367,-0.000176678256206242,
5.92280607763768));
#9478=CARTESIAN_POINT('Ctrl Pts',(-0.867511729419428,-0.341824865852328,
5.94660339370044));
#9479=CARTESIAN_POINT('Ctrl Pts',(-0.720944780593085,-0.574681060925877,
5.96564071682787));
#9480=CARTESIAN_POINT('Ctrl Pts',(-0.526555141270467,-0.769375552079073,
5.98467700523746));
#9481=CARTESIAN_POINT('Ctrl Pts',(-0.210870756052851,-0.921475670946048,
6.00846936790163));
#9482=CARTESIAN_POINT('Ctrl Pts',(0.209506448294534,-0.921438779399368,
6.03701193615958));
#9483=CARTESIAN_POINT('Ctrl Pts',(0.588220824730041,-0.739083885420811,
6.0655428661009));
#9484=CARTESIAN_POINT('Ctrl Pts',(0.849810718286318,-0.410765395052392,
6.09405857275419));
#9485=CARTESIAN_POINT('Ctrl Pts',(0.95427567990068,0.0440511715684175,6.12572236137368));
#9486=CARTESIAN_POINT('Ctrl Pts',(0.799967960952214,0.54314825140328,6.16052078866217));
#9487=CARTESIAN_POINT('Ctrl Pts',(0.354946991113063,0.898546473402006,6.19843574858538));
#9488=CARTESIAN_POINT('Ctrl Pts',(-0.212199085766547,0.940684954588202,
6.23629684514792));
#9489=CARTESIAN_POINT('Ctrl Pts',(-0.703732454340991,0.656671161576527,
6.27409476897982));
#9490=CARTESIAN_POINT('Ctrl Pts',(-0.949639640621547,0.146281182681,6.31182133692065));
#9491=CARTESIAN_POINT('Ctrl Pts',(-0.862200374710721,-0.436390813484725,
6.35103882924841));
#9492=CARTESIAN_POINT('Ctrl Pts',(-0.424615550503731,-0.87396308504598,
6.39172839424829));
#9493=CARTESIAN_POINT('Ctrl Pts',(0.140875049279472,-0.936660006455991,
6.42918239638723));
#9494=CARTESIAN_POINT('Ctrl Pts',(0.574670287621894,-0.727011014446981,
6.46186903203473));
#9495=CARTESIAN_POINT('Ctrl Pts',(0.83093266790137,-0.405200393190354,6.48982632103455));
#9496=CARTESIAN_POINT('Ctrl Pts',(0.938317766588939,0.0623494789078903,
6.52236975513327));
#9497=CARTESIAN_POINT('Ctrl Pts',(0.752579540678534,0.594055251251905,6.55945509994811));
#9498=CARTESIAN_POINT('Ctrl Pts',(0.217059284541729,0.929973502219806,6.60101727981861));
#9499=CARTESIAN_POINT('Ctrl Pts',(-0.408026785252189,0.859019100893442,
6.6424136299843));
#9500=CARTESIAN_POINT('Ctrl Pts',(-0.850845977716372,0.415638179906151,
6.68363494790014));
#9501=CARTESIAN_POINT('Ctrl Pts',(-0.920184777472661,-0.204329024249146,
6.72467349392044));
#9502=CARTESIAN_POINT('Ctrl Pts',(-0.589428074185655,-0.729814282912527,
6.76552142650441));
#9503=CARTESIAN_POINT('Ctrl Pts',(-0.00604978450581677,-0.933394312826398,
6.80617154371966));
#9504=CARTESIAN_POINT('Ctrl Pts',(0.57404869025302,-0.72985742835735,6.84661700406497));
#9505=CARTESIAN_POINT('Ctrl Pts',(0.898783211561984,-0.211649435517353,
6.8868516259356));
#9506=CARTESIAN_POINT('Ctrl Pts',(0.830853561486015,0.392570978289185,6.92686564614092));
#9507=CARTESIAN_POINT('Ctrl Pts',(0.402102843122056,0.820171632165624,6.96666187541315));
#9508=CARTESIAN_POINT('Ctrl Pts',(-0.128752136760593,0.87885181573823,7.0018337119622));
#9509=CARTESIAN_POINT('Ctrl Pts',(-0.534933891924655,0.682185839564183,
7.03245541763881));
#9510=CARTESIAN_POINT('Ctrl Pts',(-0.774943785493673,0.381327511531892,
7.05860032562784));
#9511=CARTESIAN_POINT('Ctrl Pts',(-0.859966110515312,0.00734177845082202,
7.08463607645075));
#9512=CARTESIAN_POINT('Ctrl Pts',(-0.774831422913684,-0.364904312674865,
7.11056853328824));
#9513=CARTESIAN_POINT('Ctrl Pts',(-0.537583138232402,-0.662143756003773,
7.13639250543407));
#9514=CARTESIAN_POINT('Ctrl Pts',(-0.196279169025999,-0.826362279426242,
7.16211006197668));
#9515=CARTESIAN_POINT('Ctrl Pts',(0.180788904256726,-0.82607059745876,7.18771480491698));
#9516=CARTESIAN_POINT('Ctrl Pts',(0.519038634180724,-0.662978803853832,
7.21321277550856));
#9517=CARTESIAN_POINT('Ctrl Pts',(0.751978439186691,-0.370613914749894,
7.23860036966167));
#9518=CARTESIAN_POINT('Ctrl Pts',(0.834701683971329,-0.00754650688657486,
7.26387733624003));
#9519=CARTESIAN_POINT('Ctrl Pts',(0.751920252216622,0.353483451503403,7.28904368273798));
#9520=CARTESIAN_POINT('Ctrl Pts',(0.483730036422595,0.690590593695916,7.31827398545647));
#9521=CARTESIAN_POINT('Ctrl Pts',(0.00742785048027893,0.857265989116031,
7.35149921639049));
#9522=CARTESIAN_POINT('Ctrl Pts',(-0.525293231887737,0.670073438058683,
7.38862588821794));
#9523=CARTESIAN_POINT('Ctrl Pts',(-0.822869944746703,0.195197072733832,
7.42550481928346));
#9524=CARTESIAN_POINT('Ctrl Pts',(-0.759959606004209,-0.358130855720698,
7.46213543363099));
#9525=CARTESIAN_POINT('Ctrl Pts',(-0.368415214766548,-0.748693330694505,
7.49852208898732));
#9526=CARTESIAN_POINT('Ctrl Pts',(0.177541916017237,-0.809855769006471,
7.53466251134493));
#9527=CARTESIAN_POINT('Ctrl Pts',(0.639295990646259,-0.518615892317653,
7.57056942797824));
#9528=CARTESIAN_POINT('Ctrl Pts',(0.758201052838224,-0.178255309934477,
7.59433715581631));
#9529=CARTESIAN_POINT('Ctrl Pts',(0.758224108327783,-0.00736708650145173,
7.60620065587956));
#9530=CARTESIAN_POINT('Ctrl Pts',(0.829918995390605,0.00692962491070555,
5.30024010712383));
#9531=CARTESIAN_POINT('Ctrl Pts',(0.829893790259993,0.193750817013165,5.31320971482039));
#9532=CARTESIAN_POINT('Ctrl Pts',(0.699822285583035,0.566145381882556,5.3392101566049));
#9533=CARTESIAN_POINT('Ctrl Pts',(0.195323515234371,0.88416117171195,5.37842883489126));
#9534=CARTESIAN_POINT('Ctrl Pts',(-0.400343151138505,0.817346474568011,
5.41785865980122));
#9535=CARTESIAN_POINT('Ctrl Pts',(-0.826817727686594,0.391700174990477,
5.4574958434249));
#9536=CARTESIAN_POINT('Ctrl Pts',(-0.895091678603364,-0.210180305596499,
5.49733544534094));
#9537=CARTESIAN_POINT('Ctrl Pts',(-0.571783532988076,-0.72574941013594,
5.53737192540201));
#9538=CARTESIAN_POINT('Ctrl Pts',(0.00554627097635579,-0.928352383739425,
5.57760056939562));
#9539=CARTESIAN_POINT('Ctrl Pts',(0.477799679854192,-0.76307476144334,5.61052921806703));
#9540=CARTESIAN_POINT('Ctrl Pts',(0.729410852594162,-0.490616169914011,
5.63605789108779));
#9541=CARTESIAN_POINT('Ctrl Pts',(0.881919476817548,-0.175979128010471,
5.66013043243701));
#9542=CARTESIAN_POINT('Ctrl Pts',(0.881906152444497,0.277265930526209,5.69030700929344));
#9543=CARTESIAN_POINT('Ctrl Pts',(0.600514890488868,0.690886371812261,5.72362170442843));
#9544=CARTESIAN_POINT('Ctrl Pts',(0.196921477412404,0.884675277260858,5.75399952860311));
#9545=CARTESIAN_POINT('Ctrl Pts',(-0.206656190820974,0.885009407611865,
5.78140796402136));
#9546=CARTESIAN_POINT('Ctrl Pts',(-0.571352525906284,0.709312471916405,
5.80888598178339));
#9547=CARTESIAN_POINT('Ctrl Pts',(-0.824322784093117,0.39228222278969,5.8364255516956));
#9548=CARTESIAN_POINT('Ctrl Pts',(-0.914955919505048,-0.00412326864883124,
5.86402777825679));
#9549=CARTESIAN_POINT('Ctrl Pts',(-0.839394814319228,-0.335102288993869,
5.88707765903504));
#9550=CARTESIAN_POINT('Ctrl Pts',(-0.697194784237861,-0.561053925833896,
5.90554855730548));
#9551=CARTESIAN_POINT('Ctrl Pts',(-0.508394551716055,-0.75017609097147,
5.9240379575655));
#9552=CARTESIAN_POINT('Ctrl Pts',(-0.201331843767861,-0.89822223947356,
5.94717992736717));
#9553=CARTESIAN_POINT('Ctrl Pts',(0.208503775368862,-0.898293333883727,
5.97500361673599));
#9554=CARTESIAN_POINT('Ctrl Pts',(0.578566181754719,-0.72022509709185,6.00287494476189));
#9555=CARTESIAN_POINT('Ctrl Pts',(0.834785028018541,-0.398807815817064,
6.03079323532));
#9556=CARTESIAN_POINT('Ctrl Pts',(0.937421618538533,0.0474693145637866,
6.06185942553353));
#9557=CARTESIAN_POINT('Ctrl Pts',(0.785808706512713,0.53858289651246,6.09609235737173));
#9558=CARTESIAN_POINT('Ctrl Pts',(0.346833476768302,0.889498241929319,6.13350258691761));
#9559=CARTESIAN_POINT('Ctrl Pts',(-0.214450953963022,0.931459250732699,
6.17096335002368));
#9560=CARTESIAN_POINT('Ctrl Pts',(-0.702523232936964,0.649744126672763,
6.20847735887153));
#9561=CARTESIAN_POINT('Ctrl Pts',(-0.947620032703892,0.141637172177686,
6.24603852533507));
#9562=CARTESIAN_POINT('Ctrl Pts',(-0.860569087705711,-0.440346323520561,
6.28520072180747));
#9563=CARTESIAN_POINT('Ctrl Pts',(-0.422417509108382,-0.879011958721694,
6.32595508450303));
#9564=CARTESIAN_POINT('Ctrl Pts',(0.146053510149855,-0.942361769529175,
6.36359784749923));
#9565=CARTESIAN_POINT('Ctrl Pts',(0.583529811691089,-0.731092224974979,
6.39655251871174));
#9566=CARTESIAN_POINT('Ctrl Pts',(0.842579028174264,-0.405926837413371,
6.42480144817265));
#9567=CARTESIAN_POINT('Ctrl Pts',(0.951487177832284,0.0675991994034292,
6.45775864234018));
#9568=CARTESIAN_POINT('Ctrl Pts',(0.763141746082221,0.607725575505774,6.49541116932488));
#9569=CARTESIAN_POINT('Ctrl Pts',(0.217574487524898,0.950392778021499,6.53775763542001));
#9570=CARTESIAN_POINT('Ctrl Pts',(-0.42166740973873,0.878191572890031,6.58007504544765));
#9571=CARTESIAN_POINT('Ctrl Pts',(-0.876250398231941,0.423545215383675,
6.62235503675604));
#9572=CARTESIAN_POINT('Ctrl Pts',(-0.947987096499237,-0.21459643925478,
6.6645859298645));
#9573=CARTESIAN_POINT('Ctrl Pts',(-0.606705076713124,-0.757473932422971,
6.70675774894366));
#9574=CARTESIAN_POINT('Ctrl Pts',(-0.00241202776964925,-0.968727997454768,
6.74885991888449));
#9575=CARTESIAN_POINT('Ctrl Pts',(0.600624482148029,-0.757509613558942,
6.79088237303874));
#9576=CARTESIAN_POINT('Ctrl Pts',(0.939452177122731,-0.217421016410473,
6.8328144749144));
#9577=CARTESIAN_POINT('Ctrl Pts',(0.868758799747721,0.414536277515111,6.87465507197778));
#9578=CARTESIAN_POINT('Ctrl Pts',(0.419290549746345,0.863247184920627,6.91637647714826));
#9579=CARTESIAN_POINT('Ctrl Pts',(-0.139084650191804,0.925265402913614,
6.95335818017224));
#9580=CARTESIAN_POINT('Ctrl Pts',(-0.567454545740675,0.717965354424563,
6.98564100520883));
#9581=CARTESIAN_POINT('Ctrl Pts',(-0.821064769263926,0.400211556185252,
7.0132490098583));
#9582=CARTESIAN_POINT('Ctrl Pts',(-0.91112933929112,0.00438963293201363,
7.04080231652177));
#9583=CARTESIAN_POINT('Ctrl Pts',(-0.820966778853315,-0.390275853878312,
7.0682856755789));
#9584=CARTESIAN_POINT('Ctrl Pts',(-0.569057996064222,-0.706001271167066,
7.09570447796615));
#9585=CARTESIAN_POINT('Ctrl Pts',(-0.206027274734066,-0.880764451318613,
7.1230513221731));
#9586=CARTESIAN_POINT('Ctrl Pts',(0.195812674813625,-0.880515195886687,
7.15033395522949));
#9587=CARTESIAN_POINT('Ctrl Pts',(0.556847139748695,-0.706517914293179,
7.17753857633508));
#9588=CARTESIAN_POINT('Ctrl Pts',(0.805895709935206,-0.394032847218828,
7.20466842663578));
#9589=CARTESIAN_POINT('Ctrl Pts',(0.894511398596212,-0.00535918267020315,
7.2317212151674));
#9590=CARTESIAN_POINT('Ctrl Pts',(0.805810304168001,0.381721934163946,7.25869451527825));
#9591=CARTESIAN_POINT('Ctrl Pts',(0.517921324180488,0.743697104768732,7.29007024661223));
#9592=CARTESIAN_POINT('Ctrl Pts',(0.00578604455006559,0.923078227892816,
7.32578329054371));
#9593=CARTESIAN_POINT('Ctrl Pts',(-0.568243145767641,0.721567999099011,
7.3657709938243));
#9594=CARTESIAN_POINT('Ctrl Pts',(-0.889554950114489,0.209118291781916,
7.40555959496073));
#9595=CARTESIAN_POINT('Ctrl Pts',(-0.821710123582801,-0.38904286980981,
7.44514503289073));
#9596=CARTESIAN_POINT('Ctrl Pts',(-0.397947019918738,-0.811956407468429,
7.48452302388204));
#9597=CARTESIAN_POINT('Ctrl Pts',(0.193792979174468,-0.878334837234862,
7.52368670026048));
#9598=CARTESIAN_POINT('Ctrl Pts',(0.694889984053186,-0.562420176620936,
7.56263844726097));
#9599=CARTESIAN_POINT('Ctrl Pts',(0.823996878593897,-0.192605752293447,
7.58845159102269));
#9600=CARTESIAN_POINT('Ctrl Pts',(0.824021914564924,-0.00703811992170032,
7.60133417341575));
#9601=CARTESIAN_POINT('Ctrl Pts',(0.799999065628721,0.00692558823944229,
5.30024010712383));
#9602=CARTESIAN_POINT('Ctrl Pts',(0.799974755250737,0.187114846749742,5.31274930893178));
#9603=CARTESIAN_POINT('Ctrl Pts',(0.674578200671659,0.546127076651831,5.33781512365923));
#9604=CARTESIAN_POINT('Ctrl Pts',(0.187998995393781,0.852903359039399,5.37564381521248));
#9605=CARTESIAN_POINT('Ctrl Pts',(-0.386721866921525,0.788448388841122,
5.41368605209984));
#9606=CARTESIAN_POINT('Ctrl Pts',(-0.7983994419892,0.377627224111744,5.45194644400096));
#9607=CARTESIAN_POINT('Ctrl Pts',(-0.864375113399524,-0.203617876612744,
5.49042055747836));
#9608=CARTESIAN_POINT('Ctrl Pts',(-0.552019639313923,-0.701812288635587,
5.52910737914477));
#9609=CARTESIAN_POINT('Ctrl Pts',(0.00615426428515267,-0.897757418326962,
5.56800374230524));
#9610=CARTESIAN_POINT('Ctrl Pts',(0.463089276607972,-0.737891299975203,
5.59986549204054));
#9611=CARTESIAN_POINT('Ctrl Pts',(0.706662565433678,-0.474149107376678,
5.62457829573124));
#9612=CARTESIAN_POINT('Ctrl Pts',(0.854347338563578,-0.169471123140589,
5.6478904398873));
#9613=CARTESIAN_POINT('Ctrl Pts',(0.854381411403854,0.269671075667267,5.67712918390586));
#9614=CARTESIAN_POINT('Ctrl Pts',(0.581578462406747,0.670744438556907,5.70943359497258));
#9615=CARTESIAN_POINT('Ctrl Pts',(0.189982000930166,0.858805851522918,5.73891161848027));
#9616=CARTESIAN_POINT('Ctrl Pts',(-0.201854620920769,0.859148371452269,
5.76552549972421));
#9617=CARTESIAN_POINT('Ctrl Pts',(-0.556170302204947,0.688486751453872,
5.79222147180784));
#9618=CARTESIAN_POINT('Ctrl Pts',(-0.802120584542054,0.380288702719923,
5.81899788702529));
#9619=CARTESIAN_POINT('Ctrl Pts',(-0.890321102734134,-0.0053444036833259,
5.84585301727138));
#9620=CARTESIAN_POINT('Ctrl Pts',(-0.816781798992104,-0.327577127496462,
5.86829638740099));
#9621=CARTESIAN_POINT('Ctrl Pts',(-0.678277859648778,-0.547664335405585,
5.88628859994389));
#9622=CARTESIAN_POINT('Ctrl Pts',(-0.494316135451619,-0.731945478665225,
5.90430550175064));
#9623=CARTESIAN_POINT('Ctrl Pts',(-0.194941007989142,-0.876310026230692,
5.92687230420244));
#9624=CARTESIAN_POINT('Ctrl Pts',(0.204945568353256,-0.876409485122255,
5.95402353339188));
#9625=CARTESIAN_POINT('Ctrl Pts',(0.566325487118899,-0.702556101088839,
5.98124373289334));
#9626=CARTESIAN_POINT('Ctrl Pts',(0.816751045229916,-0.388463305588866,
6.00853075028047));
#9627=CARTESIAN_POINT('Ctrl Pts',(0.917174982875959,0.0480250206861584,
6.03892142694837));
#9628=CARTESIAN_POINT('Ctrl Pts',(0.768829350780382,0.528866010776267,6.07244001895545));
#9629=CARTESIAN_POINT('Ctrl Pts',(0.338627495917749,0.872873034891815,6.10911095186911));
#9630=CARTESIAN_POINT('Ctrl Pts',(-0.212178222814091,0.914151313349766,
6.14588130840082));
#9631=CARTESIAN_POINT('Ctrl Pts',(-0.691759933067223,0.637451614256161,
6.18274515756461));
#9632=CARTESIAN_POINT('Ctrl Pts',(-0.932934482256533,0.137697594997002,
6.21969639210087));
#9633=CARTESIAN_POINT('Ctrl Pts',(-0.84730393945114,-0.435496308403701,
6.25827178793966));
#9634=CARTESIAN_POINT('Ctrl Pts',(-0.415273257958933,-0.868240176171726,
6.29847623644814));
#9635=CARTESIAN_POINT('Ctrl Pts',(0.146189896678077,-0.930950222024402,
6.33566388079779));
#9636=CARTESIAN_POINT('Ctrl Pts',(0.578787425776111,-0.722091726547751,
6.36825221458814));
#9637=CARTESIAN_POINT('Ctrl Pts',(0.835229259505866,-0.400278931762148,
6.3962159259868));
#9638=CARTESIAN_POINT('Ctrl Pts',(0.943177486850013,0.0688606453452641,
6.42887288667825));
#9639=CARTESIAN_POINT('Ctrl Pts',(0.756462512495389,0.604750444420971,6.46623690685835));
#9640=CARTESIAN_POINT('Ctrl Pts',(0.214509054547464,0.945343920852135,6.50831791566041));
#9641=CARTESIAN_POINT('Ctrl Pts',(-0.421585054233784,0.873670673138226,
6.55043539297339));
#9642=CARTESIAN_POINT('Ctrl Pts',(-0.874725713994987,0.420703846750279,
6.59257924943873));
#9643=CARTESIAN_POINT('Ctrl Pts',(-0.946491736933492,-0.216206220818672,
6.63473932973225));
#9644=CARTESIAN_POINT('Ctrl Pts',(-0.605472064685913,-0.758979181442101,
6.67690544450194));
#9645=CARTESIAN_POINT('Ctrl Pts',(-0.000509641250504898,-0.970641038681315,
6.71906739492544));
#9646=CARTESIAN_POINT('Ctrl Pts',(0.604236817182525,-0.758999928674301,
6.76121498571335));
#9647=CARTESIAN_POINT('Ctrl Pts',(0.944676427167983,-0.216670516455945,
6.80333805746961));
#9648=CARTESIAN_POINT('Ctrl Pts',(0.873719648783539,0.418956634979468,6.8454265042638));
#9649=CARTESIAN_POINT('Ctrl Pts',(0.421037273012308,0.871132652579719,6.88747029453994));
#9650=CARTESIAN_POINT('Ctrl Pts',(-0.142342851291253,0.933831870869633,
6.92479402146672));
#9651=CARTESIAN_POINT('Ctrl Pts',(-0.575104466317865,0.724476767443434,
6.95741054274359));
#9652=CARTESIAN_POINT('Ctrl Pts',(-0.831597121038275,0.403171008458228,
6.98533606563364));
#9653=CARTESIAN_POINT('Ctrl Pts',(-0.922808904665035,0.00254068286457492,
7.01322724854536));
#9654=CARTESIAN_POINT('Ctrl Pts',(-0.831484359832733,-0.397369041930912,
7.04108128388358));
#9655=CARTESIAN_POINT('Ctrl Pts',(-0.576024516479058,-0.717622866946566,
7.06889539860548));
#9656=CARTESIAN_POINT('Ctrl Pts',(-0.207464718971416,-0.895095126308869,
7.09666685370961));
#9657=CARTESIAN_POINT('Ctrl Pts',(0.200869050822812,-0.894893573965507,
7.12439296344474));
#9658=CARTESIAN_POINT('Ctrl Pts',(0.568135301656786,-0.717941543510051,
7.15207107099507));
#9659=CARTESIAN_POINT('Ctrl Pts',(0.821742493579341,-0.399813712939291,
7.17969857736332));
#9660=CARTESIAN_POINT('Ctrl Pts',(0.912100647381109,-0.00372699171446918,
7.20727292857109));
#9661=CARTESIAN_POINT('Ctrl Pts',(0.821667160899362,0.391120281113409,7.23479162069698));
#9662=CARTESIAN_POINT('Ctrl Pts',(0.527798142032111,0.760706416566583,7.26682897888736));
#9663=CARTESIAN_POINT('Ctrl Pts',(0.00437094025093319,0.944184514671381,
7.30334225024583));
#9664=CARTESIAN_POINT('Ctrl Pts',(-0.583164611559206,0.738086874931468,
7.3442757526392));
#9665=CARTESIAN_POINT('Ctrl Pts',(-0.912546668924433,0.213026529714121,
7.38505770065783));
#9666=CARTESIAN_POINT('Ctrl Pts',(-0.843060529623956,-0.400706652853849,
7.42568118182012));
#9667=CARTESIAN_POINT('Ctrl Pts',(-0.407835437985135,-0.835237258109269,
7.46613873367218));
#9668=CARTESIAN_POINT('Ctrl Pts',(0.200737244244076,-0.903598468057941,
7.5064251969444));
#9669=CARTESIAN_POINT('Ctrl Pts',(0.71672352100227,-0.578479045751934,7.54653146106904));
#9670=CARTESIAN_POINT('Ctrl Pts',(0.849917343436364,-0.197265324952655,
7.57314919120958));
#9671=CARTESIAN_POINT('Ctrl Pts',(0.849943147209423,-0.00600671278230411,
7.58642685605973));
#9672=CARTESIAN_POINT('',(0.799999065628721,0.00692558823944227,5.30024010712383));
#9673=CARTESIAN_POINT('Origin',(0.8,-5.53479071733669E-17,5.4));
#9674=CARTESIAN_POINT('',(0.849943147209423,-0.00600671278230414,7.58642685605973));
#9675=CARTESIAN_POINT('Ctrl Pts',(0.799999065628721,0.00692558823944229,
5.30024010712383));
#9676=CARTESIAN_POINT('Ctrl Pts',(0.799974755250737,0.187114846749742,5.31274930893178));
#9677=CARTESIAN_POINT('Ctrl Pts',(0.674578200671659,0.546127076651831,5.33781512365923));
#9678=CARTESIAN_POINT('Ctrl Pts',(0.187998995393781,0.852903359039399,5.37564381521248));
#9679=CARTESIAN_POINT('Ctrl Pts',(-0.386721866921525,0.788448388841122,
5.41368605209984));
#9680=CARTESIAN_POINT('Ctrl Pts',(-0.7983994419892,0.377627224111744,5.45194644400096));
#9681=CARTESIAN_POINT('Ctrl Pts',(-0.864375113399524,-0.203617876612744,
5.49042055747836));
#9682=CARTESIAN_POINT('Ctrl Pts',(-0.552019639313923,-0.701812288635587,
5.52910737914477));
#9683=CARTESIAN_POINT('Ctrl Pts',(0.00615426428515267,-0.897757418326962,
5.56800374230524));
#9684=CARTESIAN_POINT('Ctrl Pts',(0.463089276607972,-0.737891299975203,
5.59986549204054));
#9685=CARTESIAN_POINT('Ctrl Pts',(0.706662565433678,-0.474149107376678,
5.62457829573124));
#9686=CARTESIAN_POINT('Ctrl Pts',(0.854347338563578,-0.169471123140589,
5.6478904398873));
#9687=CARTESIAN_POINT('Ctrl Pts',(0.854381411403854,0.269671075667267,5.67712918390586));
#9688=CARTESIAN_POINT('Ctrl Pts',(0.581578462406747,0.670744438556907,5.70943359497258));
#9689=CARTESIAN_POINT('Ctrl Pts',(0.189982000930166,0.858805851522918,5.73891161848027));
#9690=CARTESIAN_POINT('Ctrl Pts',(-0.201854620920769,0.859148371452269,
5.76552549972421));
#9691=CARTESIAN_POINT('Ctrl Pts',(-0.556170302204947,0.688486751453872,
5.79222147180784));
#9692=CARTESIAN_POINT('Ctrl Pts',(-0.802120584542054,0.380288702719923,
5.81899788702529));
#9693=CARTESIAN_POINT('Ctrl Pts',(-0.890321102734134,-0.0053444036833259,
5.84585301727138));
#9694=CARTESIAN_POINT('Ctrl Pts',(-0.816781798992104,-0.327577127496462,
5.86829638740099));
#9695=CARTESIAN_POINT('Ctrl Pts',(-0.678277859648778,-0.547664335405585,
5.88628859994389));
#9696=CARTESIAN_POINT('Ctrl Pts',(-0.494316135451619,-0.731945478665225,
5.90430550175064));
#9697=CARTESIAN_POINT('Ctrl Pts',(-0.194941007989142,-0.876310026230692,
5.92687230420244));
#9698=CARTESIAN_POINT('Ctrl Pts',(0.204945568353256,-0.876409485122255,
5.95402353339188));
#9699=CARTESIAN_POINT('Ctrl Pts',(0.566325487118899,-0.702556101088839,
5.98124373289334));
#9700=CARTESIAN_POINT('Ctrl Pts',(0.816751045229916,-0.388463305588866,
6.00853075028047));
#9701=CARTESIAN_POINT('Ctrl Pts',(0.917174982875959,0.0480250206861584,
6.03892142694837));
#9702=CARTESIAN_POINT('Ctrl Pts',(0.768829350780382,0.528866010776267,6.07244001895545));
#9703=CARTESIAN_POINT('Ctrl Pts',(0.338627495917749,0.872873034891815,6.10911095186911));
#9704=CARTESIAN_POINT('Ctrl Pts',(-0.212178222814091,0.914151313349766,
6.14588130840082));
#9705=CARTESIAN_POINT('Ctrl Pts',(-0.691759933067223,0.637451614256161,
6.18274515756461));
#9706=CARTESIAN_POINT('Ctrl Pts',(-0.932934482256533,0.137697594997002,
6.21969639210087));
#9707=CARTESIAN_POINT('Ctrl Pts',(-0.84730393945114,-0.435496308403701,
6.25827178793966));
#9708=CARTESIAN_POINT('Ctrl Pts',(-0.415273257958933,-0.868240176171726,
6.29847623644814));
#9709=CARTESIAN_POINT('Ctrl Pts',(0.146189896678077,-0.930950222024402,
6.33566388079779));
#9710=CARTESIAN_POINT('Ctrl Pts',(0.578787425776111,-0.722091726547751,
6.36825221458814));
#9711=CARTESIAN_POINT('Ctrl Pts',(0.835229259505866,-0.400278931762148,
6.3962159259868));
#9712=CARTESIAN_POINT('Ctrl Pts',(0.943177486850013,0.0688606453452641,
6.42887288667825));
#9713=CARTESIAN_POINT('Ctrl Pts',(0.756462512495389,0.604750444420971,6.46623690685835));
#9714=CARTESIAN_POINT('Ctrl Pts',(0.214509054547464,0.945343920852135,6.50831791566041));
#9715=CARTESIAN_POINT('Ctrl Pts',(-0.421585054233784,0.873670673138226,
6.55043539297339));
#9716=CARTESIAN_POINT('Ctrl Pts',(-0.874725713994987,0.420703846750279,
6.59257924943873));
#9717=CARTESIAN_POINT('Ctrl Pts',(-0.946491736933492,-0.216206220818672,
6.63473932973225));
#9718=CARTESIAN_POINT('Ctrl Pts',(-0.605472064685913,-0.758979181442101,
6.67690544450194));
#9719=CARTESIAN_POINT('Ctrl Pts',(-0.000509641250504898,-0.970641038681315,
6.71906739492544));
#9720=CARTESIAN_POINT('Ctrl Pts',(0.604236817182525,-0.758999928674301,
6.76121498571335));
#9721=CARTESIAN_POINT('Ctrl Pts',(0.944676427167983,-0.216670516455945,
6.80333805746961));
#9722=CARTESIAN_POINT('Ctrl Pts',(0.873719648783539,0.418956634979468,6.8454265042638));
#9723=CARTESIAN_POINT('Ctrl Pts',(0.421037273012308,0.871132652579719,6.88747029453994));
#9724=CARTESIAN_POINT('Ctrl Pts',(-0.142342851291253,0.933831870869633,
6.92479402146672));
#9725=CARTESIAN_POINT('Ctrl Pts',(-0.575104466317865,0.724476767443434,
6.95741054274359));
#9726=CARTESIAN_POINT('Ctrl Pts',(-0.831597121038275,0.403171008458228,
6.98533606563364));
#9727=CARTESIAN_POINT('Ctrl Pts',(-0.922808904665035,0.00254068286457492,
7.01322724854536));
#9728=CARTESIAN_POINT('Ctrl Pts',(-0.831484359832733,-0.397369041930912,
7.04108128388358));
#9729=CARTESIAN_POINT('Ctrl Pts',(-0.576024516479058,-0.717622866946566,
7.06889539860548));
#9730=CARTESIAN_POINT('Ctrl Pts',(-0.207464718971416,-0.895095126308869,
7.09666685370961));
#9731=CARTESIAN_POINT('Ctrl Pts',(0.200869050822812,-0.894893573965507,
7.12439296344474));
#9732=CARTESIAN_POINT('Ctrl Pts',(0.568135301656786,-0.717941543510051,
7.15207107099507));
#9733=CARTESIAN_POINT('Ctrl Pts',(0.821742493579341,-0.399813712939291,
7.17969857736332));
#9734=CARTESIAN_POINT('Ctrl Pts',(0.912100647381109,-0.00372699171446918,
7.20727292857109));
#9735=CARTESIAN_POINT('Ctrl Pts',(0.821667160899362,0.391120281113409,7.23479162069698));
#9736=CARTESIAN_POINT('Ctrl Pts',(0.527798142032111,0.760706416566583,7.26682897888736));
#9737=CARTESIAN_POINT('Ctrl Pts',(0.00437094025093319,0.944184514671381,
7.30334225024583));
#9738=CARTESIAN_POINT('Ctrl Pts',(-0.583164611559206,0.738086874931468,
7.3442757526392));
#9739=CARTESIAN_POINT('Ctrl Pts',(-0.912546668924433,0.213026529714121,
7.38505770065783));
#9740=CARTESIAN_POINT('Ctrl Pts',(-0.843060529623956,-0.400706652853849,
7.42568118182012));
#9741=CARTESIAN_POINT('Ctrl Pts',(-0.407835437985135,-0.835237258109269,
7.46613873367218));
#9742=CARTESIAN_POINT('Ctrl Pts',(0.200737244244076,-0.903598468057941,
7.5064251969444));
#9743=CARTESIAN_POINT('Ctrl Pts',(0.71672352100227,-0.578479045751934,7.54653146106904));
#9744=CARTESIAN_POINT('Ctrl Pts',(0.849917343436364,-0.197265324952655,
7.57314919120958));
#9745=CARTESIAN_POINT('Ctrl Pts',(0.849943147209423,-0.00600671278230411,
7.58642685605973));
#9746=CARTESIAN_POINT('Origin',(0.799999999999999,-1.22124532708767E-15,
7.5));
#9747=CARTESIAN_POINT('Origin',(0.799999999999999,-1.22124532708767E-15,
7.5));
#9748=CARTESIAN_POINT('Origin',(0.8,-5.53479071733669E-17,5.4));
#9749=CARTESIAN_POINT('',(0.,0.,0.));
#9750=CARTESIAN_POINT('Origin',(0.,0.,7.2));
#9751=CARTESIAN_POINT('',(-0.6,-7.34788079488412E-17,7.6));
#9752=CARTESIAN_POINT('Origin',(0.,0.,7.6));
#9753=CARTESIAN_POINT('',(-0.6,-7.34788079488412E-17,6.8));
#9754=CARTESIAN_POINT('',(-0.6,-7.34788079488412E-17,7.2));
#9755=CARTESIAN_POINT('Origin',(0.,0.,6.8));
#9756=CARTESIAN_POINT('Origin',(0.,0.,6.8));
#9757=CARTESIAN_POINT('Origin',(0.,0.,7.6));
#9758=CARTESIAN_POINT('',(-1.2,-1.46957615897682E-16,8.));
#9759=CARTESIAN_POINT('Origin',(0.,0.,8.));
#9760=CARTESIAN_POINT('',(-1.2,-1.46957615897682E-16,7.6));
#9761=CARTESIAN_POINT('',(-1.2,-1.46957615897682E-16,7.6));
#9762=CARTESIAN_POINT('Origin',(0.,0.,7.6));
#9763=CARTESIAN_POINT('Origin',(0.,0.,8.));
#9764=CARTESIAN_POINT('Origin',(0.,0.,7.6));
#9765=CARTESIAN_POINT('',(0.,0.,0.));
#9766=CARTESIAN_POINT('Origin',(0.,0.,8.));
#9767=CARTESIAN_POINT('',(-0.4,-4.89858719658941E-17,11.));
#9768=CARTESIAN_POINT('Origin',(0.,0.,11.));
#9769=CARTESIAN_POINT('',(-0.4,-4.89858719658941E-17,8.));
#9770=CARTESIAN_POINT('',(-0.4,-4.89858719658941E-17,8.));
#9771=CARTESIAN_POINT('Origin',(0.,0.,8.));
#9772=CARTESIAN_POINT('Origin',(0.,0.,11.));
#9773=CARTESIAN_POINT('Origin',(0.,0.,8.));
#9774=CARTESIAN_POINT('',(0.,0.,0.));
#9775=CARTESIAN_POINT('Origin',(0.,0.39,11.));
#9776=CARTESIAN_POINT('',(-0.088881944173156,0.39,10.8609856122554));
#9777=CARTESIAN_POINT('',(-0.088881944173156,0.39,11.1390143877446));
#9778=CARTESIAN_POINT('',(-0.088881944173156,0.39,10.5));
#9779=CARTESIAN_POINT('',(-0.165,0.39,11.));
#9780=CARTESIAN_POINT('Origin',(0.,0.39,11.));
#9781=CARTESIAN_POINT('Origin',(0.,0.39,11.));
#9782=CARTESIAN_POINT('Origin',(0.,0.39,11.));
#9783=CARTESIAN_POINT('',(0.088881944173156,0.39,10.8609856122554));
#9784=CARTESIAN_POINT('Ctrl Pts',(0.088881944173156,0.39,10.8609856122554));
#9785=CARTESIAN_POINT('Ctrl Pts',(0.0808964434200154,0.391819914954193,
10.8558799045395));
#9786=CARTESIAN_POINT('Ctrl Pts',(0.072364333302368,0.393502517883282,10.8514036081398));
#9787=CARTESIAN_POINT('Ctrl Pts',(0.0431949313468624,0.398191715532106,
10.8392437758303));
#9788=CARTESIAN_POINT('Ctrl Pts',(0.0209808024963256,0.4,10.835));
#9789=CARTESIAN_POINT('Ctrl Pts',(-0.0209808024963256,0.4,10.835));
#9790=CARTESIAN_POINT('Ctrl Pts',(-0.0431949313468624,0.398191715532106,
10.8392437758303));
#9791=CARTESIAN_POINT('Ctrl Pts',(-0.072364333302368,0.393502517883282,
10.8514036081398));
#9792=CARTESIAN_POINT('Ctrl Pts',(-0.0808964434200154,0.391819914954193,
10.8558799045395));
#9793=CARTESIAN_POINT('Ctrl Pts',(-0.088881944173156,0.39,10.8609856122554));
#9794=CARTESIAN_POINT('',(0.088881944173156,0.39,11.1390143877446));
#9795=CARTESIAN_POINT('Origin',(0.,0.39,11.));
#9796=CARTESIAN_POINT('Ctrl Pts',(-0.088881944173156,0.39,11.1390143877446));
#9797=CARTESIAN_POINT('Ctrl Pts',(-0.0808964434200154,0.391819914954193,
11.1441200954605));
#9798=CARTESIAN_POINT('Ctrl Pts',(-0.072364333302368,0.393502517883282,
11.1485963918602));
#9799=CARTESIAN_POINT('Ctrl Pts',(-0.0431949313468623,0.398191715532106,
11.1607562241697));
#9800=CARTESIAN_POINT('Ctrl Pts',(-0.0209808024963255,0.4,11.165));
#9801=CARTESIAN_POINT('Ctrl Pts',(0.0209808024963256,0.4,11.165));
#9802=CARTESIAN_POINT('Ctrl Pts',(0.0431949313468623,0.398191715532106,
11.1607562241697));
#9803=CARTESIAN_POINT('Ctrl Pts',(0.072364333302368,0.393502517883282,11.1485963918602));
#9804=CARTESIAN_POINT('Ctrl Pts',(0.0808964434200153,0.391819914954193,
11.1441200954605));
#9805=CARTESIAN_POINT('Ctrl Pts',(0.088881944173156,0.39,11.1390143877446));
#9806=CARTESIAN_POINT('',(-0.165,1.49089738077441,11.));
#9807=CARTESIAN_POINT('',(-0.165,0.39,11.));
#9808=CARTESIAN_POINT('Ctrl Pts',(-0.165,1.49089738077441,11.));
#9809=CARTESIAN_POINT('Ctrl Pts',(-0.165,1.49089738077441,10.979264160895));
#9810=CARTESIAN_POINT('Ctrl Pts',(-0.160852499025073,1.49137458218466,10.9571577290991));
#9811=CARTESIAN_POINT('Ctrl Pts',(-0.144008447160944,1.49309518705251,10.916510155069));
#9812=CARTESIAN_POINT('Ctrl Pts',(-0.131312810193433,1.49431341615515,10.8979675724019));
#9813=CARTESIAN_POINT('Ctrl Pts',(-0.102032500700889,1.49659781052539,10.8686872629093));
#9814=CARTESIAN_POINT('Ctrl Pts',(-0.0834898860986569,1.49781281581157,
10.8559915687804));
#9815=CARTESIAN_POINT('Ctrl Pts',(-0.042842204593242,1.49952603771524,10.8391474746158));
#9816=CARTESIAN_POINT('Ctrl Pts',(-0.0207357355648686,1.5,10.835));
#9817=CARTESIAN_POINT('Ctrl Pts',(0.0207357355648686,1.5,10.835));
#9818=CARTESIAN_POINT('Ctrl Pts',(0.0428422045932419,1.49952603771524,10.8391474746158));
#9819=CARTESIAN_POINT('Ctrl Pts',(0.0834898860986569,1.49781281581157,10.8559915687804));
#9820=CARTESIAN_POINT('Ctrl Pts',(0.102032500700889,1.49659781052539,10.8686872629093));
#9821=CARTESIAN_POINT('Ctrl Pts',(0.131312810193433,1.49431341615515,10.8979675724019));
#9822=CARTESIAN_POINT('Ctrl Pts',(0.144008447160944,1.49309518705251,10.916510155069));
#9823=CARTESIAN_POINT('Ctrl Pts',(0.160852499025073,1.49137458218466,10.9571577290991));
#9824=CARTESIAN_POINT('Ctrl Pts',(0.165,1.49089738077441,10.979264160895));
#9825=CARTESIAN_POINT('Ctrl Pts',(0.165,1.49089738077441,11.020735839105));
#9826=CARTESIAN_POINT('Ctrl Pts',(0.160852499025073,1.49137458218466,11.0428422709009));
#9827=CARTESIAN_POINT('Ctrl Pts',(0.144008447160944,1.49309518705251,11.083489844931));
#9828=CARTESIAN_POINT('Ctrl Pts',(0.131312810193433,1.49431341615515,11.1020324275981));
#9829=CARTESIAN_POINT('Ctrl Pts',(0.102032500700889,1.49659781052539,11.1313127370907));
#9830=CARTESIAN_POINT('Ctrl Pts',(0.0834898860986569,1.49781281581157,11.1440084312196));
#9831=CARTESIAN_POINT('Ctrl Pts',(0.042842204593242,1.49952603771524,11.1608525253842));
#9832=CARTESIAN_POINT('Ctrl Pts',(0.0207357355648686,1.5,11.165));
#9833=CARTESIAN_POINT('Ctrl Pts',(-0.0207357355648686,1.5,11.165));
#9834=CARTESIAN_POINT('Ctrl Pts',(-0.0428422045932419,1.49952603771524,
11.1608525253842));
#9835=CARTESIAN_POINT('Ctrl Pts',(-0.0834898860986569,1.49781281581157,
11.1440084312196));
#9836=CARTESIAN_POINT('Ctrl Pts',(-0.102032500700889,1.49659781052539,11.1313127370907));
#9837=CARTESIAN_POINT('Ctrl Pts',(-0.131312810193433,1.49431341615515,11.1020324275981));
#9838=CARTESIAN_POINT('Ctrl Pts',(-0.144008447160944,1.49309518705251,11.083489844931));
#9839=CARTESIAN_POINT('Ctrl Pts',(-0.160852499025073,1.49137458218466,11.0428422709009));
#9840=CARTESIAN_POINT('Ctrl Pts',(-0.165,1.49089738077441,11.020735839105));
#9841=CARTESIAN_POINT('Ctrl Pts',(-0.165,1.49089738077441,11.));
#9842=CARTESIAN_POINT('Origin',(0.,0.39,11.));
#9843=CARTESIAN_POINT('',(0.088881944173156,0.39,10.5));
#9844=CARTESIAN_POINT('Origin',(0.,0.,10.5));
#9845=CARTESIAN_POINT('',(-0.4,-4.89858719658941E-17,11.5));
#9846=CARTESIAN_POINT('Origin',(0.,0.,11.5));
#9847=CARTESIAN_POINT('',(-0.4,-4.89858719658941E-17,10.5));
#9848=CARTESIAN_POINT('',(-0.4,-4.89858719658941E-17,10.5));
#9849=CARTESIAN_POINT('Origin',(0.,0.,10.5));
#9850=CARTESIAN_POINT('Origin',(0.,0.,10.5));
#9851=CARTESIAN_POINT('',(-1.5,-1.83697019872103E-16,11.5));
#9852=CARTESIAN_POINT('Origin',(0.,0.,11.5));
#9853=CARTESIAN_POINT('',(-1.5,-1.83697019872103E-16,10.5));
#9854=CARTESIAN_POINT('',(-1.5,-1.83697019872103E-16,10.5));
#9855=CARTESIAN_POINT('Origin',(0.,0.,10.5));
#9856=CARTESIAN_POINT('Origin',(0.,0.,11.5));
#9857=CARTESIAN_POINT('Origin',(0.,0.,10.5));
#9858=CARTESIAN_POINT('',(0.,0.,0.));
#9859=CARTESIAN_POINT('Origin',(0.375,0.5,0.));
#9860=CARTESIAN_POINT('',(-0.375,0.5,-4.59242549680257E-17));
#9861=CARTESIAN_POINT('Origin',(0.,0.5,0.));
#9862=CARTESIAN_POINT('Origin',(0.,0.475,0.));
#9863=CARTESIAN_POINT('',(-0.425,0.45,-5.20474889637625E-17));
#9864=CARTESIAN_POINT('Origin',(0.,0.45,0.));
#9865=CARTESIAN_POINT('',(-0.4,0.475,-4.89858719658941E-17));
#9866=CARTESIAN_POINT('Origin',(0.,0.24,0.));
#9867=CARTESIAN_POINT('',(-0.425,0.0299999999999998,-5.20474889637625E-17));
#9868=CARTESIAN_POINT('Origin',(0.,0.0299999999999998,0.));
#9869=CARTESIAN_POINT('',(-0.425,0.24,-5.20474889637625E-17));
#9870=CARTESIAN_POINT('Origin',(0.,0.0150000000000001,0.));
#9871=CARTESIAN_POINT('',(-0.395,4.85722573273506E-17,-4.83735485663204E-17));
#9872=CARTESIAN_POINT('Origin',(0.,0.,0.));
#9873=CARTESIAN_POINT('',(-0.41,0.0150000000000001,-5.02105187650415E-17));
#9874=CARTESIAN_POINT('Origin',(0.27,0.,0.));
#9875=CARTESIAN_POINT('',(-0.27,0.,-3.30654635769785E-17));
#9876=CARTESIAN_POINT('Origin',(0.,0.,0.));
#9877=CARTESIAN_POINT('Origin',(0.,-0.02,0.));
#9878=CARTESIAN_POINT('',(-0.24505,-0.0498999999999999,3.00099698131059E-17));
#9879=CARTESIAN_POINT('Origin',(0.,-0.0498999999999999,0.));
#9880=CARTESIAN_POINT('',(-0.26,-0.02,-3.18408167778312E-17));
#9881=CARTESIAN_POINT('Origin',(0.,-0.995,0.));
#9882=CARTESIAN_POINT('',(-0.24505,-1.95495,3.00099698131059E-17));
#9883=CARTESIAN_POINT('Origin',(0.,-1.95495,0.));
#9884=CARTESIAN_POINT('',(-0.24505,-0.995,-3.00099698131059E-17));
#9885=CARTESIAN_POINT('Origin',(0.,-1.975,0.));
#9886=CARTESIAN_POINT('',(-0.2,-2.,-2.44929359829471E-17));
#9887=CARTESIAN_POINT('Origin',(0.,-2.,0.));
#9888=CARTESIAN_POINT('',(-0.225,-1.975,-2.75545529808154E-17));
#9889=CARTESIAN_POINT('Origin',(0.,-2.,0.));
#9890=CARTESIAN_POINT('Origin',(0.115470053837925,-0.5,-0.2));
#9891=CARTESIAN_POINT('',(0.23094010767585,-0.5,0.));
#9892=CARTESIAN_POINT('',(0.115470053837925,-0.5,-0.2));
#9893=CARTESIAN_POINT('',(0.23094010767585,-0.5,0.));
#9894=CARTESIAN_POINT('',(0.115470053837925,-0.8,-0.2));
#9895=CARTESIAN_POINT('',(0.115470053837925,-0.5,-0.2));
#9896=CARTESIAN_POINT('',(0.23094010767585,-0.8,0.));
#9897=CARTESIAN_POINT('',(0.23094010767585,-0.8,0.));
#9898=CARTESIAN_POINT('',(0.23094010767585,-0.5,0.));
#9899=CARTESIAN_POINT('Origin',(-0.115470053837925,-0.5,-0.2));
#9900=CARTESIAN_POINT('',(-0.115470053837925,-0.5,-0.2));
#9901=CARTESIAN_POINT('',(0.115470053837925,-0.5,-0.2));
#9902=CARTESIAN_POINT('',(-0.115470053837925,-0.8,-0.2));
#9903=CARTESIAN_POINT('',(-0.115470053837925,-0.5,-0.2));
#9904=CARTESIAN_POINT('',(0.115470053837925,-0.8,-0.2));
#9905=CARTESIAN_POINT('Origin',(-0.23094010767585,-0.5,-2.77555756156289E-17));
#9906=CARTESIAN_POINT('',(-0.23094010767585,-0.5,-2.82820063659975E-17));
#9907=CARTESIAN_POINT('',(-0.115470053837925,-0.5,-0.2));
#9908=CARTESIAN_POINT('',(-0.23094010767585,-0.8,-2.77555756156289E-17));
#9909=CARTESIAN_POINT('',(-0.23094010767585,-0.5,-2.82820063659975E-17));
#9910=CARTESIAN_POINT('',(-0.115470053837925,-0.8,-0.2));
#9911=CARTESIAN_POINT('Origin',(-0.115470053837925,-0.5,0.2));
#9912=CARTESIAN_POINT('',(-0.115470053837925,-0.5,0.2));
#9913=CARTESIAN_POINT('',(-0.23094010767585,-0.5,-2.82820063659975E-17));
#9914=CARTESIAN_POINT('',(-0.115470053837925,-0.8,0.2));
#9915=CARTESIAN_POINT('',(-0.115470053837925,-0.5,0.2));
#9916=CARTESIAN_POINT('',(-0.23094010767585,-0.8,-2.82820063659975E-17));
#9917=CARTESIAN_POINT('Origin',(0.115470053837925,-0.5,0.2));
#9918=CARTESIAN_POINT('',(0.115470053837925,-0.5,0.2));
#9919=CARTESIAN_POINT('',(-0.115470053837925,-0.5,0.2));
#9920=CARTESIAN_POINT('',(0.115470053837925,-0.8,0.2));
#9921=CARTESIAN_POINT('',(0.115470053837925,-0.5,0.2));
#9922=CARTESIAN_POINT('',(-0.115470053837925,-0.8,0.2));
#9923=CARTESIAN_POINT('Origin',(0.23094010767585,-0.5,0.));
#9924=CARTESIAN_POINT('',(0.115470053837925,-0.5,0.2));
#9925=CARTESIAN_POINT('',(0.115470053837925,-0.8,0.2));
#9926=CARTESIAN_POINT('Origin',(0.,-0.5,0.));
#9927=CARTESIAN_POINT('Origin',(0.,-0.8,0.));
#9928=CARTESIAN_POINT('',(0.,0.,0.));
#9929=CARTESIAN_POINT('Origin',(0.,0.,0.));
#9930=CARTESIAN_POINT('',(-0.42,0.16,5.14351655641888E-17));
#9931=CARTESIAN_POINT('Origin',(0.,0.16,0.));
#9932=CARTESIAN_POINT('',(-0.42,0.,5.14351655641888E-17));
#9933=CARTESIAN_POINT('',(-0.42,0.,5.14351655641888E-17));
#9934=CARTESIAN_POINT('Origin',(0.,0.,0.));
#9935=CARTESIAN_POINT('Origin',(0.,0.,0.));
#9936=CARTESIAN_POINT('',(-0.8,0.16,9.79717439317883E-17));
#9937=CARTESIAN_POINT('Origin',(0.,0.16,0.));
#9938=CARTESIAN_POINT('',(-0.8,0.,9.79717439317883E-17));
#9939=CARTESIAN_POINT('',(-0.8,0.,9.79717439317883E-17));
#9940=CARTESIAN_POINT('Origin',(0.,0.,0.));
#9941=CARTESIAN_POINT('Origin',(0.,0.16,0.));
#9942=CARTESIAN_POINT('Origin',(0.,0.,0.));
#9943=CARTESIAN_POINT('',(0.,0.,0.));
#9944=CARTESIAN_POINT('Origin',(0.,0.067277284513851,0.));
#9945=CARTESIAN_POINT('',(-0.375277674973257,0.0768195421087395,0.65));
#9946=CARTESIAN_POINT('',(0.375277674973257,0.0768195421087395,0.65));
#9947=CARTESIAN_POINT('Ctrl Pts',(-0.375277674973257,0.0768195421087395,
0.65));
#9948=CARTESIAN_POINT('Ctrl Pts',(1.66533453693773E-13,-0.0315137912242439,
0.65));
#9949=CARTESIAN_POINT('Ctrl Pts',(0.375277674973257,0.0768195421087394,
0.65));
#9950=CARTESIAN_POINT('',(-0.750555349946514,0.0768195421087394,-9.19165206894919E-17));
#9951=CARTESIAN_POINT('Ctrl Pts',(-0.750555349946514,0.0768195421087394,
-9.19165206894919E-17));
#9952=CARTESIAN_POINT('Ctrl Pts',(-0.562916512459802,-0.0315137912242434,
0.325000000000144));
#9953=CARTESIAN_POINT('Ctrl Pts',(-0.375277674973257,0.0768195421087395,
0.65));
#9954=CARTESIAN_POINT('',(-0.6175,-2.77555756156289E-17,-7.5621939847349E-17));
#9955=CARTESIAN_POINT('',(-0.734027674973257,0.067277284513851,-8.98924642641573E-17));
#9956=CARTESIAN_POINT('Origin',(0.,0.,0.));
#9957=CARTESIAN_POINT('',(-0.375277674973257,0.0768195421087395,-0.65));
#9958=CARTESIAN_POINT('Ctrl Pts',(-0.375277674973257,0.0768195421087395,
-0.65));
#9959=CARTESIAN_POINT('Ctrl Pts',(-0.562916512459968,-0.0315137912242437,
-0.324999999999856));
#9960=CARTESIAN_POINT('Ctrl Pts',(-0.750555349946514,0.0768195421087395,
-9.19165206894919E-17));
#9961=CARTESIAN_POINT('',(0.375277674973257,0.0768195421087395,-0.65));
#9962=CARTESIAN_POINT('Ctrl Pts',(0.375277674973257,0.0768195421087395,
-0.65));
#9963=CARTESIAN_POINT('Ctrl Pts',(-1.66144875635155E-13,-0.0315137912242437,
-0.65));
#9964=CARTESIAN_POINT('Ctrl Pts',(-0.375277674973257,0.0768195421087395,
-0.65));
#9965=CARTESIAN_POINT('',(0.750555349946514,0.0768195421087394,0.));
#9966=CARTESIAN_POINT('Ctrl Pts',(0.750555349946514,0.0768195421087394,
0.));
#9967=CARTESIAN_POINT('Ctrl Pts',(0.562916512459802,-0.0315137912242436,
-0.325000000000144));
#9968=CARTESIAN_POINT('Ctrl Pts',(0.375277674973257,0.0768195421087395,
-0.65));
#9969=CARTESIAN_POINT('Ctrl Pts',(0.375277674973257,0.0768195421087394,
0.65));
#9970=CARTESIAN_POINT('Ctrl Pts',(0.562916512459968,-0.0315137912242439,
0.324999999999856));
#9971=CARTESIAN_POINT('Ctrl Pts',(0.750555349946514,0.0768195421087394,
0.));
#9972=CARTESIAN_POINT('Origin',(0.,0.612722715486149,0.));
#9973=CARTESIAN_POINT('',(-0.6175,0.68,-7.5621939847349E-17));
#9974=CARTESIAN_POINT('Origin',(0.,0.68,0.));
#9975=CARTESIAN_POINT('',(-0.750555349946514,0.603180457891261,-9.19165206894919E-17));
#9976=CARTESIAN_POINT('',(-0.734027674973257,0.612722715486149,-8.98924642641573E-17));
#9977=CARTESIAN_POINT('',(-0.375277674973257,0.603180457891261,0.65));
#9978=CARTESIAN_POINT('Ctrl Pts',(-0.375277674973257,0.603180457891261,
0.65));
#9979=CARTESIAN_POINT('Ctrl Pts',(-0.562916512459968,0.711513791224243,
0.324999999999856));
#9980=CARTESIAN_POINT('Ctrl Pts',(-0.750555349946514,0.603180457891261,
-9.19165206894919E-17));
#9981=CARTESIAN_POINT('',(0.375277674973257,0.603180457891261,0.65));
#9982=CARTESIAN_POINT('Ctrl Pts',(0.375277674973257,0.603180457891261,0.65));
#9983=CARTESIAN_POINT('Ctrl Pts',(-1.66755498298699E-13,0.711513791224244,
0.65));
#9984=CARTESIAN_POINT('Ctrl Pts',(-0.375277674973257,0.603180457891261,
0.65));
#9985=CARTESIAN_POINT('',(0.750555349946514,0.603180457891261,0.));
#9986=CARTESIAN_POINT('Ctrl Pts',(0.750555349946514,0.603180457891261,0.));
#9987=CARTESIAN_POINT('Ctrl Pts',(0.562916512459802,0.711513791224244,0.325000000000144));
#9988=CARTESIAN_POINT('Ctrl Pts',(0.375277674973257,0.603180457891261,0.65));
#9989=CARTESIAN_POINT('',(0.375277674973257,0.603180457891261,-0.65));
#9990=CARTESIAN_POINT('Ctrl Pts',(0.375277674973257,0.603180457891261,-0.65));
#9991=CARTESIAN_POINT('Ctrl Pts',(0.562916512459969,0.711513791224244,-0.324999999999856));
#9992=CARTESIAN_POINT('Ctrl Pts',(0.750555349946514,0.603180457891261,0.));
#9993=CARTESIAN_POINT('',(-0.375277674973257,0.603180457891261,-0.65));
#9994=CARTESIAN_POINT('Ctrl Pts',(-0.375277674973257,0.603180457891261,
-0.65));
#9995=CARTESIAN_POINT('Ctrl Pts',(1.66422431391311E-13,0.711513791224244,
-0.65));
#9996=CARTESIAN_POINT('Ctrl Pts',(0.375277674973257,0.603180457891261,-0.65));
#9997=CARTESIAN_POINT('Ctrl Pts',(-0.750555349946514,0.603180457891261,
-9.19165206894919E-17));
#9998=CARTESIAN_POINT('Ctrl Pts',(-0.562916512459802,0.711513791224244,
-0.325000000000144));
#9999=CARTESIAN_POINT('Ctrl Pts',(-0.375277674973257,0.603180457891261,
-0.65));
#10000=CARTESIAN_POINT('Origin',(0.375277674973257,0.,-0.65));
#10001=CARTESIAN_POINT('',(-0.375277674973257,0.,-0.65));
#10002=CARTESIAN_POINT('',(0.375277674973257,0.,-0.65));
#10003=CARTESIAN_POINT('Origin',(-0.375277674973257,0.,-0.65));
#10004=CARTESIAN_POINT('',(-0.750555349946514,0.,-9.19165206894919E-17));
#10005=CARTESIAN_POINT('Origin',(-0.750555349946514,0.,-9.19165206894919E-17));
#10006=CARTESIAN_POINT('',(-0.375277674973257,0.,0.65));
#10007=CARTESIAN_POINT('Origin',(0.,0.,0.));
#10008=CARTESIAN_POINT('',(-0.338975,0.68,4.15124648740974E-17));
#10009=CARTESIAN_POINT('Origin',(0.,0.68,0.));
#10010=CARTESIAN_POINT('',(-0.338975,0.,4.15124648740974E-17));
#10011=CARTESIAN_POINT('',(-0.338975,0.,4.15124648740974E-17));
#10012=CARTESIAN_POINT('Origin',(0.,0.,0.));
#10013=CARTESIAN_POINT('Origin',(-0.375277674973257,0.,0.65));
#10014=CARTESIAN_POINT('',(0.375277674973257,0.,0.65));
#10015=CARTESIAN_POINT('Origin',(0.750555349946514,0.,0.));
#10016=CARTESIAN_POINT('',(0.750555349946514,0.,0.));
#10017=CARTESIAN_POINT('Origin',(0.375277674973257,0.,0.65));
#10018=CARTESIAN_POINT('Origin',(0.,0.68,-1.11022302462516E-16));
#10019=CARTESIAN_POINT('Origin',(0.,0.,-1.11022302462516E-16));
#10020=CARTESIAN_POINT('',(0.,0.,0.));
#10021=CARTESIAN_POINT('Origin',(0.0577350269189626,0.,-0.1));
#10022=CARTESIAN_POINT('',(0.0577350269189626,0.,-0.1));
#10023=CARTESIAN_POINT('',(0.115470053837925,0.,0.));
#10024=CARTESIAN_POINT('',(0.0934187836487032,0.,-0.0381939203391614));
#10025=CARTESIAN_POINT('',(0.0577350269189626,-0.2,-0.1));
#10026=CARTESIAN_POINT('',(0.0577350269189626,0.,-0.1));
#10027=CARTESIAN_POINT('',(0.115470053837925,-0.2,0.));
#10028=CARTESIAN_POINT('',(0.115470053837925,-0.2,0.));
#10029=CARTESIAN_POINT('',(0.115470053837925,0.,0.));
#10030=CARTESIAN_POINT('Origin',(-0.0577350269189626,0.,-0.1));
#10031=CARTESIAN_POINT('',(-0.0577350269189626,0.,-0.1));
#10032=CARTESIAN_POINT('',(0.0561324865405187,0.,-0.1));
#10033=CARTESIAN_POINT('',(-0.0577350269189626,-0.2,-0.1));
#10034=CARTESIAN_POINT('',(-0.0577350269189626,0.,-0.1));
#10035=CARTESIAN_POINT('',(0.0577350269189626,-0.2,-0.1));
#10036=CARTESIAN_POINT('Origin',(-0.115470053837925,0.,-1.38777878078145E-17));
#10037=CARTESIAN_POINT('',(-0.115470053837925,0.,-1.41410031829988E-17));
#10038=CARTESIAN_POINT('',(-0.0797862971081845,0.,-0.0618060796608387));
#10039=CARTESIAN_POINT('',(-0.115470053837925,-0.2,-1.38777878078145E-17));
#10040=CARTESIAN_POINT('',(-0.115470053837925,0.,-1.41410031829988E-17));
#10041=CARTESIAN_POINT('',(-0.0577350269189626,-0.2,-0.1));
#10042=CARTESIAN_POINT('Origin',(-0.0577350269189626,0.,0.1));
#10043=CARTESIAN_POINT('',(-0.0577350269189626,0.,0.1));
#10044=CARTESIAN_POINT('',(-0.0509187836487033,0.,0.111806079660839));
#10045=CARTESIAN_POINT('',(-0.0577350269189626,-0.2,0.1));
#10046=CARTESIAN_POINT('',(-0.0577350269189626,0.,0.1));
#10047=CARTESIAN_POINT('',(-0.115470053837925,-0.2,-1.41410031829988E-17));
#10048=CARTESIAN_POINT('Origin',(0.0577350269189626,0.,0.1));
#10049=CARTESIAN_POINT('',(0.0577350269189626,0.,0.1));
#10050=CARTESIAN_POINT('',(0.113867513459481,0.,0.1));
#10051=CARTESIAN_POINT('',(0.0577350269189626,-0.2,0.1));
#10052=CARTESIAN_POINT('',(0.0577350269189626,0.,0.1));
#10053=CARTESIAN_POINT('',(-0.0577350269189626,-0.2,0.1));
#10054=CARTESIAN_POINT('Origin',(0.115470053837925,0.,0.));
#10055=CARTESIAN_POINT('',(0.122286297108185,0.,-0.0118060796608386));
#10056=CARTESIAN_POINT('',(0.0577350269189626,-0.2,0.1));
#10057=CARTESIAN_POINT('Origin',(0.,-0.2,0.));
#10058=CARTESIAN_POINT('Origin',(0.17,0.,0.));
#10059=CARTESIAN_POINT('',(-0.17,-8.67361737988404E-18,-2.0818995585505E-17));
#10060=CARTESIAN_POINT('Origin',(0.,0.,0.));
#10061=CARTESIAN_POINT('Origin',(0.,-0.015,0.));
#10062=CARTESIAN_POINT('',(-0.1954,-0.0254,-2.39295984553393E-17));
#10063=CARTESIAN_POINT('Origin',(0.,-0.0254,0.));
#10064=CARTESIAN_POINT('',(-0.185,-0.015,-2.2655965784226E-17));
#10065=CARTESIAN_POINT('Origin',(0.,-0.2775,0.));
#10066=CARTESIAN_POINT('',(-0.1954,-0.5296,2.39295984553393E-17));
#10067=CARTESIAN_POINT('Origin',(0.,-0.5296,0.));
#10068=CARTESIAN_POINT('',(-0.1954,-0.2775,-2.39295984553393E-17));
#10069=CARTESIAN_POINT('Origin',(0.,-0.5625,0.));
#10070=CARTESIAN_POINT('',(-0.125,-0.6,-1.53080849893419E-17));
#10071=CARTESIAN_POINT('Origin',(0.,-0.6,0.));
#10072=CARTESIAN_POINT('',(-0.1625,-0.5625,-1.99005104861445E-17));
#10073=CARTESIAN_POINT('Origin',(0.,-0.6,0.));
#10074=CARTESIAN_POINT('',(0.,0.,0.));
#10075=CARTESIAN_POINT('Origin',(0.,0.,0.));
#10076=CARTESIAN_POINT('',(-7.57444045272638E-17,-1.60428730688303E-17,
0.6185));
#10077=CARTESIAN_POINT('Origin',(-9.17872775960941E-17,0.,0.7495));
#10078=CARTESIAN_POINT('Origin',(0.,1.60428730688303E-17,0.));
#10079=CARTESIAN_POINT('',(0.,0.,0.));
#10080=CARTESIAN_POINT('Origin',(0.,-3.,0.5));
#10081=CARTESIAN_POINT('',(-0.225,-3.,0.6));
#10082=CARTESIAN_POINT('Origin',(0.,-3.,0.6));
#10083=CARTESIAN_POINT('',(-0.225,-3.,1.));
#10084=CARTESIAN_POINT('',(-0.225,-3.,0.5));
#10085=CARTESIAN_POINT('Origin',(0.,-3.,1.));
#10086=CARTESIAN_POINT('Origin',(1.,-2.2,0.6));
#10087=CARTESIAN_POINT('',(1.,-2.2,0.6));
#10088=CARTESIAN_POINT('',(-1.,-2.2,0.6));
#10089=CARTESIAN_POINT('',(1.,-2.2,0.6));
#10090=CARTESIAN_POINT('',(-1.,-2.2,1.));
#10091=CARTESIAN_POINT('',(-1.,-2.2,0.6));
#10092=CARTESIAN_POINT('',(1.,-2.2,1.));
#10093=CARTESIAN_POINT('',(1.,-2.2,1.));
#10094=CARTESIAN_POINT('',(1.,-2.2,0.6));
#10095=CARTESIAN_POINT('Origin',(1.,-3.8,0.6));
#10096=CARTESIAN_POINT('',(1.,-3.8,0.6));
#10097=CARTESIAN_POINT('',(1.,-3.8,0.6));
#10098=CARTESIAN_POINT('',(1.,-3.8,1.));
#10099=CARTESIAN_POINT('',(1.,-3.8,1.));
#10100=CARTESIAN_POINT('',(1.,-3.8,0.6));
#10101=CARTESIAN_POINT('Origin',(-1.,-3.8,0.6));
#10102=CARTESIAN_POINT('',(-1.,-3.8,0.6));
#10103=CARTESIAN_POINT('',(-1.,-3.8,0.6));
#10104=CARTESIAN_POINT('',(-1.,-3.8,1.));
#10105=CARTESIAN_POINT('',(-1.,-3.8,1.));
#10106=CARTESIAN_POINT('',(-1.,-3.8,0.6));
#10107=CARTESIAN_POINT('Origin',(-1.,-2.2,0.6));
#10108=CARTESIAN_POINT('',(-1.,-2.2,0.6));
#10109=CARTESIAN_POINT('',(-1.,-2.2,1.));
#10110=CARTESIAN_POINT('Origin',(0.,-3.,1.));
#10111=CARTESIAN_POINT('Origin',(0.,-3.,0.6));
#10112=CARTESIAN_POINT('',(0.,0.,0.));
#10113=CARTESIAN_POINT('Origin',(0.3,0.4,0.));
#10114=CARTESIAN_POINT('',(-0.3,0.4,-3.67394039744206E-17));
#10115=CARTESIAN_POINT('Origin',(0.,0.4,0.));
#10116=CARTESIAN_POINT('Origin',(0.,0.375,0.));
#10117=CARTESIAN_POINT('',(-0.35,0.35,-4.28626379701573E-17));
#10118=CARTESIAN_POINT('Origin',(0.,0.35,0.));
#10119=CARTESIAN_POINT('',(-0.325,0.375,-3.9801020972289E-17));
#10120=CARTESIAN_POINT('Origin',(0.,0.19,0.));
#10121=CARTESIAN_POINT('',(-0.35,0.03,-4.28626379701574E-17));
#10122=CARTESIAN_POINT('Origin',(0.,0.03,0.));
#10123=CARTESIAN_POINT('',(-0.35,0.19,-4.28626379701574E-17));
#10124=CARTESIAN_POINT('Origin',(0.,0.0149999999999999,0.));
#10125=CARTESIAN_POINT('',(-0.32,-3.29597460435593E-17,-3.91886975727153E-17));
#10126=CARTESIAN_POINT('Origin',(0.,0.,0.));
#10127=CARTESIAN_POINT('',(-0.335,0.0149999999999999,-4.10256677714363E-17));
#10128=CARTESIAN_POINT('Origin',(0.22,0.,0.));
#10129=CARTESIAN_POINT('',(-0.22,-6.93889390390723E-18,-2.69422295812418E-17));
#10130=CARTESIAN_POINT('Origin',(0.,0.,0.));
#10131=CARTESIAN_POINT('Origin',(0.,-0.02,0.));
#10132=CARTESIAN_POINT('',(-0.1954,-0.0492,2.39295984553393E-17));
#10133=CARTESIAN_POINT('Origin',(0.,-0.0492,0.));
#10134=CARTESIAN_POINT('',(-0.21,-0.02,-2.57175827820944E-17));
#10135=CARTESIAN_POINT('Origin',(0.,-0.8,0.));
#10136=CARTESIAN_POINT('',(-0.1954,-1.5646,2.39295984553393E-17));
#10137=CARTESIAN_POINT('Origin',(0.,-1.5646,0.));
#10138=CARTESIAN_POINT('',(-0.1954,-0.8,-2.39295984553393E-17));
#10139=CARTESIAN_POINT('Origin',(0.,-1.58,0.));
#10140=CARTESIAN_POINT('',(-0.16,-1.6,-1.95943487863577E-17));
#10141=CARTESIAN_POINT('Origin',(0.,-1.6,0.));
#10142=CARTESIAN_POINT('',(-0.18,-1.58,-2.20436423846524E-17));
#10143=CARTESIAN_POINT('Origin',(0.,-1.6,0.));
#10144=CARTESIAN_POINT('Origin',(0.0866025403784439,-0.4,-0.15));
#10145=CARTESIAN_POINT('',(0.173205080756888,-0.4,0.));
#10146=CARTESIAN_POINT('',(0.0866025403784439,-0.4,-0.15));
#10147=CARTESIAN_POINT('',(0.173205080756888,-0.4,0.));
#10148=CARTESIAN_POINT('',(0.0866025403784439,-0.64,-0.15));
#10149=CARTESIAN_POINT('',(0.0866025403784439,-0.4,-0.15));
#10150=CARTESIAN_POINT('',(0.173205080756888,-0.64,0.));
#10151=CARTESIAN_POINT('',(0.173205080756888,-0.64,0.));
#10152=CARTESIAN_POINT('',(0.173205080756888,-0.4,0.));
#10153=CARTESIAN_POINT('Origin',(-0.0866025403784438,-0.4,-0.15));
#10154=CARTESIAN_POINT('',(-0.0866025403784438,-0.4,-0.15));
#10155=CARTESIAN_POINT('',(0.0866025403784439,-0.4,-0.15));
#10156=CARTESIAN_POINT('',(-0.0866025403784438,-0.64,-0.15));
#10157=CARTESIAN_POINT('',(-0.0866025403784438,-0.4,-0.15));
#10158=CARTESIAN_POINT('',(0.0866025403784439,-0.64,-0.15));
#10159=CARTESIAN_POINT('Origin',(-0.173205080756888,-0.4,-2.77555756156289E-17));
#10160=CARTESIAN_POINT('',(-0.173205080756888,-0.4,-2.12115047744981E-17));
#10161=CARTESIAN_POINT('',(-0.0866025403784438,-0.4,-0.15));
#10162=CARTESIAN_POINT('',(-0.173205080756888,-0.64,-2.77555756156289E-17));
#10163=CARTESIAN_POINT('',(-0.173205080756888,-0.4,-2.12115047744981E-17));
#10164=CARTESIAN_POINT('',(-0.0866025403784438,-0.64,-0.15));
#10165=CARTESIAN_POINT('Origin',(-0.0866025403784439,-0.4,0.15));
#10166=CARTESIAN_POINT('',(-0.0866025403784439,-0.4,0.15));
#10167=CARTESIAN_POINT('',(-0.173205080756888,-0.4,-2.12115047744981E-17));
#10168=CARTESIAN_POINT('',(-0.0866025403784439,-0.64,0.15));
#10169=CARTESIAN_POINT('',(-0.0866025403784439,-0.4,0.15));
#10170=CARTESIAN_POINT('',(-0.173205080756888,-0.64,-2.12115047744981E-17));
#10171=CARTESIAN_POINT('Origin',(0.0866025403784439,-0.4,0.15));
#10172=CARTESIAN_POINT('',(0.0866025403784439,-0.4,0.15));
#10173=CARTESIAN_POINT('',(-0.0866025403784439,-0.4,0.15));
#10174=CARTESIAN_POINT('',(0.0866025403784439,-0.64,0.15));
#10175=CARTESIAN_POINT('',(0.0866025403784439,-0.4,0.15));
#10176=CARTESIAN_POINT('',(-0.0866025403784439,-0.64,0.15));
#10177=CARTESIAN_POINT('Origin',(0.173205080756888,-0.4,0.));
#10178=CARTESIAN_POINT('',(0.0866025403784439,-0.4,0.15));
#10179=CARTESIAN_POINT('',(0.0866025403784439,-0.64,0.15));
#10180=CARTESIAN_POINT('Origin',(0.,-0.4,-2.77555756156289E-17));
#10181=CARTESIAN_POINT('Origin',(0.,-0.64,-2.77555756156289E-17));
#10182=CARTESIAN_POINT('',(0.,0.,0.));
#10183=CARTESIAN_POINT('',(0.,0.,0.));
#10184=CARTESIAN_POINT('',(0.,0.,0.));
#10185=CARTESIAN_POINT('',(0.,0.,0.));
#10186=CARTESIAN_POINT('',(0.,0.,0.));
#10187=CARTESIAN_POINT('',(-5.,0.,2.3));
#10188=CARTESIAN_POINT('',(5.,0.,3.9));
#10189=CARTESIAN_POINT('',(0.,0.,0.));
#10190=CARTESIAN_POINT('',(0.,0.,0.));
#10191=CARTESIAN_POINT('',(0.,0.,0.));
#10192=CARTESIAN_POINT('',(0.,0.,0.));
#10193=CARTESIAN_POINT('',(0.,0.,0.));
#10194=CARTESIAN_POINT('',(0.,0.,0.));
#10195=CARTESIAN_POINT('',(0.,0.,0.));
#10196=CARTESIAN_POINT('',(0.,0.,0.));
#10197=CARTESIAN_POINT('',(0.,0.,0.));
#10198=CARTESIAN_POINT('',(0.,0.,0.));
#10199=CARTESIAN_POINT('',(2.94448637286709,1.7,5.7));
#10200=CARTESIAN_POINT('',(0.,3.4,5.7));
#10201=CARTESIAN_POINT('',(-2.94448637286709,1.7,5.7));
#10202=CARTESIAN_POINT('',(-2.94448637286709,-1.7,5.7));
#10203=CARTESIAN_POINT('',(-4.44089209850063E-16,-3.4,5.7));
#10204=CARTESIAN_POINT('',(2.94448637286709,-1.7,5.7));
#10205=CARTESIAN_POINT('',(0.,0.,9.5));
#10206=CARTESIAN_POINT('',(0.,0.,9.66));
#10207=CARTESIAN_POINT('',(0.,1.,11.));
#10208=CARTESIAN_POINT('',(2.05060966544099,2.05060966544099,1.));
#10209=CARTESIAN_POINT('',(-2.05060966544099,2.05060966544099,1.));
#10210=CARTESIAN_POINT('',(-2.05060966544099,-2.05060966544099,1.));
#10211=CARTESIAN_POINT('',(2.05060966544099,-2.05060966544099,1.));
#10212=CARTESIAN_POINT('',(0.,0.,0.9));
#10213=CARTESIAN_POINT('',(-4.,3.,0.));
#10214=CARTESIAN_POINT('',(-4.,-4.44089209850063E-16,0.));
#10215=CARTESIAN_POINT('',(4.,3.,0.));
#10216=CARTESIAN_POINT('',(4.,-4.44089209850063E-16,0.));
#10217=UNCERTAINTY_MEASURE_WITH_UNIT(LENGTH_MEASURE(0.001),#10267,
'DISTANCE_ACCURACY_VALUE',
'Maximum model space distance between geometric entities at asserted c
onnectivities');
#10218=UNCERTAINTY_MEASURE_WITH_UNIT(LENGTH_MEASURE(0.001),#10267,
'DISTANCE_ACCURACY_VALUE',
'Maximum model space distance between geometric entities at asserted c
onnectivities');
#10219=UNCERTAINTY_MEASURE_WITH_UNIT(LENGTH_MEASURE(0.001),#10267,
'DISTANCE_ACCURACY_VALUE',
'Maximum model space distance between geometric entities at asserted c
onnectivities');
#10220=UNCERTAINTY_MEASURE_WITH_UNIT(LENGTH_MEASURE(0.001),#10267,
'DISTANCE_ACCURACY_VALUE',
'Maximum model space distance between geometric entities at asserted c
onnectivities');
#10221=UNCERTAINTY_MEASURE_WITH_UNIT(LENGTH_MEASURE(0.001),#10267,
'DISTANCE_ACCURACY_VALUE',
'Maximum model space distance between geometric entities at asserted c
onnectivities');
#10222=UNCERTAINTY_MEASURE_WITH_UNIT(LENGTH_MEASURE(0.001),#10267,
'DISTANCE_ACCURACY_VALUE',
'Maximum model space distance between geometric entities at asserted c
onnectivities');
#10223=UNCERTAINTY_MEASURE_WITH_UNIT(LENGTH_MEASURE(0.001),#10267,
'DISTANCE_ACCURACY_VALUE',
'Maximum model space distance between geometric entities at asserted c
onnectivities');
#10224=UNCERTAINTY_MEASURE_WITH_UNIT(LENGTH_MEASURE(0.001),#10267,
'DISTANCE_ACCURACY_VALUE',
'Maximum model space distance between geometric entities at asserted c
onnectivities');
#10225=UNCERTAINTY_MEASURE_WITH_UNIT(LENGTH_MEASURE(0.001),#10267,
'DISTANCE_ACCURACY_VALUE',
'Maximum model space distance between geometric entities at asserted c
onnectivities');
#10226=UNCERTAINTY_MEASURE_WITH_UNIT(LENGTH_MEASURE(0.001),#10267,
'DISTANCE_ACCURACY_VALUE',
'Maximum model space distance between geometric entities at asserted c
onnectivities');
#10227=UNCERTAINTY_MEASURE_WITH_UNIT(LENGTH_MEASURE(0.001),#10267,
'DISTANCE_ACCURACY_VALUE',
'Maximum model space distance between geometric entities at asserted c
onnectivities');
#10228=UNCERTAINTY_MEASURE_WITH_UNIT(LENGTH_MEASURE(0.001),#10267,
'DISTANCE_ACCURACY_VALUE',
'Maximum model space distance between geometric entities at asserted c
onnectivities');
#10229=UNCERTAINTY_MEASURE_WITH_UNIT(LENGTH_MEASURE(0.001),#10267,
'DISTANCE_ACCURACY_VALUE',
'Maximum model space distance between geometric entities at asserted c
onnectivities');
#10230=UNCERTAINTY_MEASURE_WITH_UNIT(LENGTH_MEASURE(0.001),#10267,
'DISTANCE_ACCURACY_VALUE',
'Maximum model space distance between geometric entities at asserted c
onnectivities');
#10231=UNCERTAINTY_MEASURE_WITH_UNIT(LENGTH_MEASURE(0.001),#10267,
'DISTANCE_ACCURACY_VALUE',
'Maximum model space distance between geometric entities at asserted c
onnectivities');
#10232=UNCERTAINTY_MEASURE_WITH_UNIT(LENGTH_MEASURE(0.001),#10267,
'DISTANCE_ACCURACY_VALUE',
'Maximum model space distance between geometric entities at asserted c
onnectivities');
#10233=UNCERTAINTY_MEASURE_WITH_UNIT(LENGTH_MEASURE(0.001),#10267,
'DISTANCE_ACCURACY_VALUE',
'Maximum model space distance between geometric entities at asserted c
onnectivities');
#10234=UNCERTAINTY_MEASURE_WITH_UNIT(LENGTH_MEASURE(0.001),#10267,
'DISTANCE_ACCURACY_VALUE',
'Maximum model space distance between geometric entities at asserted c
onnectivities');
#10235=UNCERTAINTY_MEASURE_WITH_UNIT(LENGTH_MEASURE(0.001),#10267,
'DISTANCE_ACCURACY_VALUE',
'Maximum model space distance between geometric entities at asserted c
onnectivities');
#10236=UNCERTAINTY_MEASURE_WITH_UNIT(LENGTH_MEASURE(0.001),#10267,
'DISTANCE_ACCURACY_VALUE',
'Maximum model space distance between geometric entities at asserted c
onnectivities');
#10237=UNCERTAINTY_MEASURE_WITH_UNIT(LENGTH_MEASURE(0.001),#10267,
'DISTANCE_ACCURACY_VALUE',
'Maximum model space distance between geometric entities at asserted c
onnectivities');
#10238=UNCERTAINTY_MEASURE_WITH_UNIT(LENGTH_MEASURE(0.001),#10267,
'DISTANCE_ACCURACY_VALUE',
'Maximum model space distance between geometric entities at asserted c
onnectivities');
#10239=UNCERTAINTY_MEASURE_WITH_UNIT(LENGTH_MEASURE(0.001),#10267,
'DISTANCE_ACCURACY_VALUE',
'Maximum model space distance between geometric entities at asserted c
onnectivities');
#10240=UNCERTAINTY_MEASURE_WITH_UNIT(LENGTH_MEASURE(0.001),#10267,
'DISTANCE_ACCURACY_VALUE',
'Maximum model space distance between geometric entities at asserted c
onnectivities');
#10241=UNCERTAINTY_MEASURE_WITH_UNIT(LENGTH_MEASURE(0.001),#10267,
'DISTANCE_ACCURACY_VALUE',
'Maximum model space distance between geometric entities at asserted c
onnectivities');
#10242=(
GEOMETRIC_REPRESENTATION_CONTEXT(3)
GLOBAL_UNCERTAINTY_ASSIGNED_CONTEXT((#10217))
GLOBAL_UNIT_ASSIGNED_CONTEXT((#10267,#10269,#10270))
REPRESENTATION_CONTEXT('','3D')
);
#10243=(
GEOMETRIC_REPRESENTATION_CONTEXT(3)
GLOBAL_UNCERTAINTY_ASSIGNED_CONTEXT((#10218))
GLOBAL_UNIT_ASSIGNED_CONTEXT((#10267,#10269,#10270))
REPRESENTATION_CONTEXT('','3D')
);
#10244=(
GEOMETRIC_REPRESENTATION_CONTEXT(3)
GLOBAL_UNCERTAINTY_ASSIGNED_CONTEXT((#10219))
GLOBAL_UNIT_ASSIGNED_CONTEXT((#10267,#10269,#10270))
REPRESENTATION_CONTEXT('','3D')
);
#10245=(
GEOMETRIC_REPRESENTATION_CONTEXT(3)
GLOBAL_UNCERTAINTY_ASSIGNED_CONTEXT((#10220))
GLOBAL_UNIT_ASSIGNED_CONTEXT((#10267,#10269,#10270))
REPRESENTATION_CONTEXT('','3D')
);
#10246=(
GEOMETRIC_REPRESENTATION_CONTEXT(3)
GLOBAL_UNCERTAINTY_ASSIGNED_CONTEXT((#10221))
GLOBAL_UNIT_ASSIGNED_CONTEXT((#10267,#10269,#10270))
REPRESENTATION_CONTEXT('','3D')
);
#10247=(
GEOMETRIC_REPRESENTATION_CONTEXT(3)
GLOBAL_UNCERTAINTY_ASSIGNED_CONTEXT((#10222))
GLOBAL_UNIT_ASSIGNED_CONTEXT((#10267,#10269,#10270))
REPRESENTATION_CONTEXT('','3D')
);
#10248=(
GEOMETRIC_REPRESENTATION_CONTEXT(3)
GLOBAL_UNCERTAINTY_ASSIGNED_CONTEXT((#10223))
GLOBAL_UNIT_ASSIGNED_CONTEXT((#10267,#10269,#10270))
REPRESENTATION_CONTEXT('','3D')
);
#10249=(
GEOMETRIC_REPRESENTATION_CONTEXT(3)
GLOBAL_UNCERTAINTY_ASSIGNED_CONTEXT((#10224))
GLOBAL_UNIT_ASSIGNED_CONTEXT((#10267,#10269,#10270))
REPRESENTATION_CONTEXT('','3D')
);
#10250=(
GEOMETRIC_REPRESENTATION_CONTEXT(3)
GLOBAL_UNCERTAINTY_ASSIGNED_CONTEXT((#10225))
GLOBAL_UNIT_ASSIGNED_CONTEXT((#10267,#10269,#10270))
REPRESENTATION_CONTEXT('','3D')
);
#10251=(
GEOMETRIC_REPRESENTATION_CONTEXT(3)
GLOBAL_UNCERTAINTY_ASSIGNED_CONTEXT((#10226))
GLOBAL_UNIT_ASSIGNED_CONTEXT((#10267,#10269,#10270))
REPRESENTATION_CONTEXT('','3D')
);
#10252=(
GEOMETRIC_REPRESENTATION_CONTEXT(3)
GLOBAL_UNCERTAINTY_ASSIGNED_CONTEXT((#10227))
GLOBAL_UNIT_ASSIGNED_CONTEXT((#10267,#10269,#10270))
REPRESENTATION_CONTEXT('','3D')
);
#10253=(
GEOMETRIC_REPRESENTATION_CONTEXT(3)
GLOBAL_UNCERTAINTY_ASSIGNED_CONTEXT((#10228))
GLOBAL_UNIT_ASSIGNED_CONTEXT((#10267,#10269,#10270))
REPRESENTATION_CONTEXT('','3D')
);
#10254=(
GEOMETRIC_REPRESENTATION_CONTEXT(3)
GLOBAL_UNCERTAINTY_ASSIGNED_CONTEXT((#10229))
GLOBAL_UNIT_ASSIGNED_CONTEXT((#10267,#10269,#10270))
REPRESENTATION_CONTEXT('','3D')
);
#10255=(
GEOMETRIC_REPRESENTATION_CONTEXT(3)
GLOBAL_UNCERTAINTY_ASSIGNED_CONTEXT((#10230))
GLOBAL_UNIT_ASSIGNED_CONTEXT((#10267,#10269,#10270))
REPRESENTATION_CONTEXT('','3D')
);
#10256=(
GEOMETRIC_REPRESENTATION_CONTEXT(3)
GLOBAL_UNCERTAINTY_ASSIGNED_CONTEXT((#10231))
GLOBAL_UNIT_ASSIGNED_CONTEXT((#10267,#10269,#10270))
REPRESENTATION_CONTEXT('','3D')
);
#10257=(
GEOMETRIC_REPRESENTATION_CONTEXT(3)
GLOBAL_UNCERTAINTY_ASSIGNED_CONTEXT((#10232))
GLOBAL_UNIT_ASSIGNED_CONTEXT((#10267,#10269,#10270))
REPRESENTATION_CONTEXT('','3D')
);
#10258=(
GEOMETRIC_REPRESENTATION_CONTEXT(3)
GLOBAL_UNCERTAINTY_ASSIGNED_CONTEXT((#10233))
GLOBAL_UNIT_ASSIGNED_CONTEXT((#10267,#10269,#10270))
REPRESENTATION_CONTEXT('','3D')
);
#10259=(
GEOMETRIC_REPRESENTATION_CONTEXT(3)
GLOBAL_UNCERTAINTY_ASSIGNED_CONTEXT((#10234))
GLOBAL_UNIT_ASSIGNED_CONTEXT((#10267,#10269,#10270))
REPRESENTATION_CONTEXT('','3D')
);
#10260=(
GEOMETRIC_REPRESENTATION_CONTEXT(3)
GLOBAL_UNCERTAINTY_ASSIGNED_CONTEXT((#10235))
GLOBAL_UNIT_ASSIGNED_CONTEXT((#10267,#10269,#10270))
REPRESENTATION_CONTEXT('','3D')
);
#10261=(
GEOMETRIC_REPRESENTATION_CONTEXT(3)
GLOBAL_UNCERTAINTY_ASSIGNED_CONTEXT((#10236))
GLOBAL_UNIT_ASSIGNED_CONTEXT((#10267,#10269,#10270))
REPRESENTATION_CONTEXT('','3D')
);
#10262=(
GEOMETRIC_REPRESENTATION_CONTEXT(3)
GLOBAL_UNCERTAINTY_ASSIGNED_CONTEXT((#10237))
GLOBAL_UNIT_ASSIGNED_CONTEXT((#10267,#10269,#10270))
REPRESENTATION_CONTEXT('','3D')
);
#10263=(
GEOMETRIC_REPRESENTATION_CONTEXT(3)
GLOBAL_UNCERTAINTY_ASSIGNED_CONTEXT((#10238))
GLOBAL_UNIT_ASSIGNED_CONTEXT((#10267,#10269,#10270))
REPRESENTATION_CONTEXT('','3D')
);
#10264=(
GEOMETRIC_REPRESENTATION_CONTEXT(3)
GLOBAL_UNCERTAINTY_ASSIGNED_CONTEXT((#10239))
GLOBAL_UNIT_ASSIGNED_CONTEXT((#10267,#10269,#10270))
REPRESENTATION_CONTEXT('','3D')
);
#10265=(
GEOMETRIC_REPRESENTATION_CONTEXT(3)
GLOBAL_UNCERTAINTY_ASSIGNED_CONTEXT((#10240))
GLOBAL_UNIT_ASSIGNED_CONTEXT((#10267,#10269,#10270))
REPRESENTATION_CONTEXT('','3D')
);
#10266=(
GEOMETRIC_REPRESENTATION_CONTEXT(3)
GLOBAL_UNCERTAINTY_ASSIGNED_CONTEXT((#10241))
GLOBAL_UNIT_ASSIGNED_CONTEXT((#10267,#10269,#10270))
REPRESENTATION_CONTEXT('','3D')
);
#10267=(
LENGTH_UNIT()
NAMED_UNIT(*)
SI_UNIT(.CENTI.,.METRE.)
);
#10268=(
LENGTH_UNIT()
NAMED_UNIT(*)
SI_UNIT($,.METRE.)
);
#10269=(
NAMED_UNIT(*)
PLANE_ANGLE_UNIT()
SI_UNIT($,.RADIAN.)
);
#10270=(
NAMED_UNIT(*)
SI_UNIT($,.STERADIAN.)
SOLID_ANGLE_UNIT()
);
#10271=SHAPE_DEFINITION_REPRESENTATION(#10295,#10354);
#10272=SHAPE_DEFINITION_REPRESENTATION(#10296,#10355);
#10273=SHAPE_DEFINITION_REPRESENTATION(#10297,#10356);
#10274=SHAPE_DEFINITION_REPRESENTATION(#10298,#10357);
#10275=SHAPE_DEFINITION_REPRESENTATION(#10299,#10358);
#10276=SHAPE_DEFINITION_REPRESENTATION(#10300,#10359);
#10277=SHAPE_DEFINITION_REPRESENTATION(#10301,#10360);
#10278=SHAPE_DEFINITION_REPRESENTATION(#10302,#10361);
#10279=SHAPE_DEFINITION_REPRESENTATION(#10303,#10362);
#10280=SHAPE_DEFINITION_REPRESENTATION(#10304,#10363);
#10281=SHAPE_DEFINITION_REPRESENTATION(#10305,#10364);
#10282=SHAPE_DEFINITION_REPRESENTATION(#10306,#10365);
#10283=SHAPE_DEFINITION_REPRESENTATION(#10307,#10366);
#10284=SHAPE_DEFINITION_REPRESENTATION(#10308,#10367);
#10285=SHAPE_DEFINITION_REPRESENTATION(#10309,#10368);
#10286=SHAPE_DEFINITION_REPRESENTATION(#10310,#10369);
#10287=SHAPE_DEFINITION_REPRESENTATION(#10311,#10370);
#10288=SHAPE_DEFINITION_REPRESENTATION(#10312,#10371);
#10289=SHAPE_DEFINITION_REPRESENTATION(#10313,#10372);
#10290=SHAPE_DEFINITION_REPRESENTATION(#10314,#10373);
#10291=SHAPE_DEFINITION_REPRESENTATION(#10315,#10374);
#10292=SHAPE_DEFINITION_REPRESENTATION(#10316,#10375);
#10293=SHAPE_DEFINITION_REPRESENTATION(#10317,#10376);
#10294=SHAPE_DEFINITION_REPRESENTATION(#10318,#10377);
#10295=PRODUCT_DEFINITION_SHAPE('',$,#10379);
#10296=PRODUCT_DEFINITION_SHAPE('',$,#10380);
#10297=PRODUCT_DEFINITION_SHAPE('',$,#10381);
#10298=PRODUCT_DEFINITION_SHAPE('',$,#10382);
#10299=PRODUCT_DEFINITION_SHAPE('',$,#10383);
#10300=PRODUCT_DEFINITION_SHAPE('',$,#10384);
#10301=PRODUCT_DEFINITION_SHAPE('',$,#10385);
#10302=PRODUCT_DEFINITION_SHAPE('',$,#10386);
#10303=PRODUCT_DEFINITION_SHAPE('',$,#10387);
#10304=PRODUCT_DEFINITION_SHAPE('',$,#10388);
#10305=PRODUCT_DEFINITION_SHAPE('',$,#10389);
#10306=PRODUCT_DEFINITION_SHAPE('',$,#10390);
#10307=PRODUCT_DEFINITION_SHAPE('',$,#10391);
#10308=PRODUCT_DEFINITION_SHAPE('',$,#10392);
#10309=PRODUCT_DEFINITION_SHAPE('',$,#10393);
#10310=PRODUCT_DEFINITION_SHAPE('',$,#10394);
#10311=PRODUCT_DEFINITION_SHAPE('',$,#10395);
#10312=PRODUCT_DEFINITION_SHAPE('',$,#10396);
#10313=PRODUCT_DEFINITION_SHAPE('',$,#10397);
#10314=PRODUCT_DEFINITION_SHAPE('',$,#10398);
#10315=PRODUCT_DEFINITION_SHAPE('',$,#10399);
#10316=PRODUCT_DEFINITION_SHAPE('',$,#10400);
#10317=PRODUCT_DEFINITION_SHAPE('',$,#10401);
#10318=PRODUCT_DEFINITION_SHAPE('',$,#10402);
#10319=PRODUCT_DEFINITION_SHAPE($,$,#116);
#10320=PRODUCT_DEFINITION_SHAPE($,$,#117);
#10321=PRODUCT_DEFINITION_SHAPE($,$,#118);
#10322=PRODUCT_DEFINITION_SHAPE($,$,#119);
#10323=PRODUCT_DEFINITION_SHAPE($,$,#120);
#10324=PRODUCT_DEFINITION_SHAPE($,$,#121);
#10325=PRODUCT_DEFINITION_SHAPE($,$,#122);
#10326=PRODUCT_DEFINITION_SHAPE($,$,#123);
#10327=PRODUCT_DEFINITION_SHAPE($,$,#124);
#10328=PRODUCT_DEFINITION_SHAPE($,$,#125);
#10329=PRODUCT_DEFINITION_SHAPE($,$,#126);
#10330=PRODUCT_DEFINITION_SHAPE($,$,#127);
#10331=PRODUCT_DEFINITION_SHAPE($,$,#128);
#10332=PRODUCT_DEFINITION_SHAPE($,$,#129);
#10333=PRODUCT_DEFINITION_SHAPE($,$,#130);
#10334=PRODUCT_DEFINITION_SHAPE($,$,#131);
#10335=PRODUCT_DEFINITION_SHAPE($,$,#132);
#10336=PRODUCT_DEFINITION_SHAPE($,$,#133);
#10337=PRODUCT_DEFINITION_SHAPE($,$,#134);
#10338=PRODUCT_DEFINITION_SHAPE($,$,#135);
#10339=PRODUCT_DEFINITION_SHAPE($,$,#136);
#10340=PRODUCT_DEFINITION_SHAPE($,$,#137);
#10341=PRODUCT_DEFINITION_SHAPE($,$,#138);
#10342=PRODUCT_DEFINITION_SHAPE($,$,#139);
#10343=PRODUCT_DEFINITION_SHAPE($,$,#140);
#10344=PRODUCT_DEFINITION_SHAPE($,$,#141);
#10345=PRODUCT_DEFINITION_SHAPE($,$,#142);
#10346=PRODUCT_DEFINITION_SHAPE($,$,#143);
#10347=PRODUCT_DEFINITION_SHAPE($,$,#144);
#10348=PRODUCT_DEFINITION_SHAPE($,$,#145);
#10349=PRODUCT_DEFINITION_SHAPE($,$,#146);
#10350=PRODUCT_DEFINITION_SHAPE($,$,#147);
#10351=PRODUCT_DEFINITION_SHAPE($,$,#148);
#10352=PRODUCT_DEFINITION_SHAPE($,$,#149);
#10353=PRODUCT_DEFINITION_SHAPE($,$,#150);
#10354=SHAPE_REPRESENTATION('',(#4970,#5521,#5522,#5523,#5524,#5525,#5526,
#5527,#5528,#5529,#5530,#5531,#5532,#5533,#5534,#5535,#5536,#5537,#5538,
#5539,#5540,#5541,#5542,#5543,#5544,#5545,#5546,#5547,#5548,#5549,#5550,
#5551,#5552,#5553,#5554,#5555),#10242);
#10355=SHAPE_REPRESENTATION('',(#4971),#10243);
#10356=SHAPE_REPRESENTATION('',(#5114),#10244);
#10357=SHAPE_REPRESENTATION('',(#5118),#10245);
#10358=SHAPE_REPRESENTATION('',(#5144),#10246);
#10359=SHAPE_REPRESENTATION('',(#5166),#10247);
#10360=SHAPE_REPRESENTATION('',(#5198),#10248);
#10361=SHAPE_REPRESENTATION('',(#5222),#10249);
#10362=SHAPE_REPRESENTATION('',(#5231),#10250);
#10363=SHAPE_REPRESENTATION('',(#5253),#10251);
#10364=SHAPE_REPRESENTATION('',(#5262),#10252);
#10365=SHAPE_REPRESENTATION('',(#5289),#10253);
#10366=SHAPE_REPRESENTATION('',(#5306),#10254);
#10367=SHAPE_REPRESENTATION('',(#5377),#10255);
#10368=SHAPE_REPRESENTATION('',(#5382),#10256);
#10369=SHAPE_REPRESENTATION('',(#5392),#10257);
#10370=SHAPE_REPRESENTATION('',(#5398),#10258);
#10371=SHAPE_REPRESENTATION('',(#5413),#10259);
#10372=SHAPE_REPRESENTATION('',(#5439),#10260);
#10373=SHAPE_REPRESENTATION('',(#5448),#10261);
#10374=SHAPE_REPRESENTATION('',(#5464),#10262);
#10375=SHAPE_REPRESENTATION('',(#5481),#10263);
#10376=SHAPE_REPRESENTATION('',(#5485),#10264);
#10377=SHAPE_REPRESENTATION('',(#5495),#10265);
#10378=PRODUCT_DEFINITION_CONTEXT('part definition',#10452,'design');
#10379=PRODUCT_DEFINITION('PAT-015',
'PAT-015',#10403,#10378);
#10380=PRODUCT_DEFINITION('Filter regulator body',
'Filter regulator body',#10404,#10378);
#10381=PRODUCT_DEFINITION('Bowl face seal','Bowl face seal',#10405,
#10378);
#10382=PRODUCT_DEFINITION('Perforated filter insert',
'Perforated filter insert',#10406,#10378);
#10383=PRODUCT_DEFINITION('Gauge dummy','Gauge dummy',#10407,
#10378);
#10384=PRODUCT_DEFINITION('Wall bracket','Wall bracket',#10408,
#10378);
#10385=PRODUCT_DEFINITION('Hex Pipe Nipple - 1-4 Inch Tapered Pipe Thread',
'Hex Pipe Nipple - 1-4 Inch Tapered Pipe Thread',#10409,#10378);
#10386=PRODUCT_DEFINITION('Valve seat','Valve seat',#10410,
#10378);
#10387=PRODUCT_DEFINITION('Poppet and stem','Poppet and stem',
#10411,#10378);
#10388=PRODUCT_DEFINITION('Lower diaphragm plate',
'Lower diaphragm plate',#10412,#10378);
#10389=PRODUCT_DEFINITION('Diaphragm','Diaphragm',#10413,
#10378);
#10390=PRODUCT_DEFINITION('Upper diaphragm plate',
'Upper diaphragm plate',#10414,#10378);
#10391=PRODUCT_DEFINITION('Bonnet','Bonnet',#10415,#10378);
#10392=PRODUCT_DEFINITION('Control spring','Control spring',
#10416,#10378);
#10393=PRODUCT_DEFINITION('Adjuster spring shoe',
'Adjuster spring shoe',#10417,#10378);
#10394=PRODUCT_DEFINITION('Adjusting screw','Adjusting screw',
#10418,#10378);
#10395=PRODUCT_DEFINITION('Adjuster knob','Adjuster knob',#10419,
#10378);
#10396=PRODUCT_DEFINITION('Cap Screw - M5x20',
'Cap Screw - M5x20',#10420,#10378);
#10397=PRODUCT_DEFINITION('Flat Washer - M8','Flat Washer - M8',
#10421,#10378);
#10398=PRODUCT_DEFINITION('Hex Nut - M8','Hex Nut - M8',#10422,
#10378);
#10399=PRODUCT_DEFINITION('Socket Set Screw - M4x6',
'Socket Set Screw - M4x6',#10423,#10378);
#10400=PRODUCT_DEFINITION('O-Ring','O-Ring',#10424,#10378);
#10401=PRODUCT_DEFINITION('Mounting foot','Mounting foot',#10425,
#10378);
#10402=PRODUCT_DEFINITION('Cap Screw - M4x16',
'Cap Screw - M4x16',#10426,#10378);
#10403=PRODUCT_DEFINITION_FORMATION('',$,#10454);
#10404=PRODUCT_DEFINITION_FORMATION('',$,#10455);
#10405=PRODUCT_DEFINITION_FORMATION('',$,#10456);
#10406=PRODUCT_DEFINITION_FORMATION('',$,#10457);
#10407=PRODUCT_DEFINITION_FORMATION('',$,#10458);
#10408=PRODUCT_DEFINITION_FORMATION('',$,#10459);
#10409=PRODUCT_DEFINITION_FORMATION('',$,#10460);
#10410=PRODUCT_DEFINITION_FORMATION('',$,#10461);
#10411=PRODUCT_DEFINITION_FORMATION('',$,#10462);
#10412=PRODUCT_DEFINITION_FORMATION('',$,#10463);
#10413=PRODUCT_DEFINITION_FORMATION('',$,#10464);
#10414=PRODUCT_DEFINITION_FORMATION('',$,#10465);
#10415=PRODUCT_DEFINITION_FORMATION('',$,#10466);
#10416=PRODUCT_DEFINITION_FORMATION('',$,#10467);
#10417=PRODUCT_DEFINITION_FORMATION('',$,#10468);
#10418=PRODUCT_DEFINITION_FORMATION('',$,#10469);
#10419=PRODUCT_DEFINITION_FORMATION('',$,#10470);
#10420=PRODUCT_DEFINITION_FORMATION('',$,#10471);
#10421=PRODUCT_DEFINITION_FORMATION('',$,#10472);
#10422=PRODUCT_DEFINITION_FORMATION('',$,#10473);
#10423=PRODUCT_DEFINITION_FORMATION('',$,#10474);
#10424=PRODUCT_DEFINITION_FORMATION('',$,#10475);
#10425=PRODUCT_DEFINITION_FORMATION('',$,#10476);
#10426=PRODUCT_DEFINITION_FORMATION('',$,#10477);
#10427=PRODUCT_RELATED_PRODUCT_CATEGORY(
'PAT-015',
'PAT-015',(#10454));
#10428=PRODUCT_RELATED_PRODUCT_CATEGORY('Filter regulator body',
'Filter regulator body',(#10455));
#10429=PRODUCT_RELATED_PRODUCT_CATEGORY('Bowl face seal',
'Bowl face seal',(#10456));
#10430=PRODUCT_RELATED_PRODUCT_CATEGORY('Perforated filter insert',
'Perforated filter insert',(#10457));
#10431=PRODUCT_RELATED_PRODUCT_CATEGORY('Gauge dummy','Gauge dummy',(#10458));
#10432=PRODUCT_RELATED_PRODUCT_CATEGORY('Wall bracket','Wall bracket',(#10459));
#10433=PRODUCT_RELATED_PRODUCT_CATEGORY(
'Hex Pipe Nipple - 1-4 Inch Tapered Pipe Thread',
'Hex Pipe Nipple - 1-4 Inch Tapered Pipe Thread',(#10460));
#10434=PRODUCT_RELATED_PRODUCT_CATEGORY('Valve seat','Valve seat',(#10461));
#10435=PRODUCT_RELATED_PRODUCT_CATEGORY('Poppet and stem',
'Poppet and stem',(#10462));
#10436=PRODUCT_RELATED_PRODUCT_CATEGORY('Lower diaphragm plate',
'Lower diaphragm plate',(#10463));
#10437=PRODUCT_RELATED_PRODUCT_CATEGORY('Diaphragm','Diaphragm',(#10464));
#10438=PRODUCT_RELATED_PRODUCT_CATEGORY('Upper diaphragm plate',
'Upper diaphragm plate',(#10465));
#10439=PRODUCT_RELATED_PRODUCT_CATEGORY('Bonnet','Bonnet',(#10466));
#10440=PRODUCT_RELATED_PRODUCT_CATEGORY('Control spring',
'Control spring',(#10467));
#10441=PRODUCT_RELATED_PRODUCT_CATEGORY('Adjuster spring shoe',
'Adjuster spring shoe',(#10468));
#10442=PRODUCT_RELATED_PRODUCT_CATEGORY('Adjusting screw',
'Adjusting screw',(#10469));
#10443=PRODUCT_RELATED_PRODUCT_CATEGORY('Adjuster knob','Adjuster knob',
(#10470));
#10444=PRODUCT_RELATED_PRODUCT_CATEGORY('Cap Screw - M5x20',
'Cap Screw - M5x20',(#10471));
#10445=PRODUCT_RELATED_PRODUCT_CATEGORY('Flat Washer - M8',
'Flat Washer - M8',(#10472));
#10446=PRODUCT_RELATED_PRODUCT_CATEGORY('Hex Nut - M8','Hex Nut - M8',(#10473));
#10447=PRODUCT_RELATED_PRODUCT_CATEGORY('Socket Set Screw - M4x6',
'Socket Set Screw - M4x6',(#10474));
#10448=PRODUCT_RELATED_PRODUCT_CATEGORY('O-Ring','O-Ring',(#10475));
#10449=PRODUCT_RELATED_PRODUCT_CATEGORY('Mounting foot','Mounting foot',
(#10476));
#10450=PRODUCT_RELATED_PRODUCT_CATEGORY('Cap Screw - M4x16',
'Cap Screw - M4x16',(#10477));
#10451=APPLICATION_PROTOCOL_DEFINITION('international standard',
'automotive_design',2009,#10452);
#10452=APPLICATION_CONTEXT(
'Core Data for Automotive Mechanical Design Process');
#10453=PRODUCT_CONTEXT('part definition',#10452,'mechanical');
#10454=PRODUCT('PAT-015',
'PAT-015',
'PAT-015',(#10453));
#10455=PRODUCT('Filter regulator body','Filter regulator body',
'Filter regulator body',(#10453));
#10456=PRODUCT('Bowl face seal','Bowl face seal',
'Bowl face seal',(#10453));
#10457=PRODUCT('Perforated filter insert','Perforated filter insert',
'Perforated filter insert',(#10453));
#10458=PRODUCT('Gauge dummy','Gauge dummy','Gauge dummy',(#10453));
#10459=PRODUCT('Wall bracket','Wall bracket',
'Wall bracket',(#10453));
#10460=PRODUCT('Hex Pipe Nipple - 1-4 Inch Tapered Pipe Thread',
'Hex Pipe Nipple - 1-4 Inch Tapered Pipe Thread',
'Hex Pipe Nipple - 1-4 Inch Tapered Pipe Thread',(#10453));
#10461=PRODUCT('Valve seat','Valve seat','Valve seat',(#10453));
#10462=PRODUCT('Poppet and stem','Poppet and stem',
'Poppet and stem',(#10453));
#10463=PRODUCT('Lower diaphragm plate','Lower diaphragm plate',
'Lower diaphragm plate',(#10453));
#10464=PRODUCT('Diaphragm','Diaphragm','Diaphragm',(#10453));
#10465=PRODUCT('Upper diaphragm plate','Upper diaphragm plate',
'Upper diaphragm plate',(#10453));
#10466=PRODUCT('Bonnet','Bonnet','Bonnet',(#10453));
#10467=PRODUCT('Control spring','Control spring',
'Control spring',(#10453));
#10468=PRODUCT('Adjuster spring shoe','Adjuster spring shoe',
'Adjuster spring shoe',(#10453));
#10469=PRODUCT('Adjusting screw','Adjusting screw',
'Adjusting screw',(#10453));
#10470=PRODUCT('Adjuster knob','Adjuster knob',
'Adjuster knob',(#10453));
#10471=PRODUCT('Cap Screw - M5x20','Cap Screw - M5x20',
'Cap Screw - M5x20',(#10453));
#10472=PRODUCT('Flat Washer - M8','Flat Washer - M8',
'Flat Washer - M8',(#10453));
#10473=PRODUCT('Hex Nut - M8','Hex Nut - M8',
'Hex Nut - M8',(#10453));
#10474=PRODUCT('Socket Set Screw - M4x6','Socket Set Screw - M4x6',
'Socket Set Screw - M4x6',(#10453));
#10475=PRODUCT('O-Ring','O-Ring','O-Ring',(#10453));
#10476=PRODUCT('Mounting foot','Mounting foot',
'Mounting foot',(#10453));
#10477=PRODUCT('Cap Screw - M4x16','Cap Screw - M4x16',
'Cap Screw - M4x16',(#10453));
#10478=PRESENTATION_STYLE_ASSIGNMENT((#10484));
#10479=PRESENTATION_STYLE_ASSIGNMENT((#10485));
#10480=PRESENTATION_STYLE_ASSIGNMENT((#10486));
#10481=PRESENTATION_STYLE_ASSIGNMENT((#10487));
#10482=PRESENTATION_STYLE_ASSIGNMENT((#10488));
#10483=PRESENTATION_STYLE_ASSIGNMENT((#10489));
#10484=SURFACE_STYLE_USAGE(.BOTH.,#10490);
#10485=SURFACE_STYLE_USAGE(.BOTH.,#10491);
#10486=SURFACE_STYLE_USAGE(.BOTH.,#10492);
#10487=SURFACE_STYLE_USAGE(.BOTH.,#10493);
#10488=SURFACE_STYLE_USAGE(.BOTH.,#10494);
#10489=SURFACE_STYLE_USAGE(.BOTH.,#10495);
#10490=SURFACE_SIDE_STYLE('',(#10496));
#10491=SURFACE_SIDE_STYLE('',(#10497));
#10492=SURFACE_SIDE_STYLE('',(#10498));
#10493=SURFACE_SIDE_STYLE('',(#10499));
#10494=SURFACE_SIDE_STYLE('',(#10500));
#10495=SURFACE_SIDE_STYLE('',(#10501));
#10496=SURFACE_STYLE_FILL_AREA(#10502);
#10497=SURFACE_STYLE_FILL_AREA(#10503);
#10498=SURFACE_STYLE_FILL_AREA(#10504);
#10499=SURFACE_STYLE_FILL_AREA(#10505);
#10500=SURFACE_STYLE_FILL_AREA(#10506);
#10501=SURFACE_STYLE_FILL_AREA(#10507);
#10502=FILL_AREA_STYLE('Steel - Satin',(#10508));
#10503=FILL_AREA_STYLE('CAD Library Painted - Engineering blue',(#10509));
#10504=FILL_AREA_STYLE('CAD Library Painted - Off white',(#10510));
#10505=FILL_AREA_STYLE('CAD Library Painted - Graphite',(#10511));
#10506=FILL_AREA_STYLE('CAD Library Painted - Steel gray',(#10512));
#10507=FILL_AREA_STYLE('CAD Library Painted - Deep blue',(#10513));
#10508=FILL_AREA_STYLE_COLOUR('Steel - Satin',#10514);
#10509=FILL_AREA_STYLE_COLOUR('CAD Library Painted - Engineering blue',
#10515);
#10510=FILL_AREA_STYLE_COLOUR('CAD Library Painted - Off white',#10516);
#10511=FILL_AREA_STYLE_COLOUR('CAD Library Painted - Graphite',#10517);
#10512=FILL_AREA_STYLE_COLOUR('CAD Library Painted - Steel gray',#10518);
#10513=FILL_AREA_STYLE_COLOUR('CAD Library Painted - Deep blue',#10519);
#10514=COLOUR_RGB('Steel - Satin',0.627450980392157,0.627450980392157,0.627450980392157);
#10515=COLOUR_RGB('CAD Library Painted - Engineering blue',0.12156862745098,
0.356862745098039,0.6);
#10516=COLOUR_RGB('CAD Library Painted - Off white',0.909803921568627,0.901960784313726,
0.858823529411765);
#10517=COLOUR_RGB('CAD Library Painted - Graphite',0.0980392156862745,0.109803921568627,
0.125490196078431);
#10518=COLOUR_RGB('CAD Library Painted - Steel gray',0.592156862745098,
0.631372549019608,0.67843137254902);
#10519=COLOUR_RGB('CAD Library Painted - Deep blue',0.0784313725490196,
0.203921568627451,0.349019607843137);
#10520=COLOUR_RGB('Dark Blue',0.08,0.2,0.34);
#10521=FILL_AREA_STYLE_COLOUR('',#10520);
#10522=FILL_AREA_STYLE('',(#10521));
#10523=SURFACE_STYLE_FILL_AREA(#10522);
#10524=SURFACE_SIDE_STYLE('',(#10523));
#10525=SURFACE_STYLE_USAGE(.BOTH.,#10524);
#10526=PRESENTATION_STYLE_ASSIGNMENT((#10525));
#10527=COLOUR_RGB('Light Blue',0.38,0.62,0.78);
#10528=FILL_AREA_STYLE_COLOUR('',#10527);
#10529=FILL_AREA_STYLE('',(#10528));
#10530=SURFACE_STYLE_FILL_AREA(#10529);
#10531=SURFACE_SIDE_STYLE('',(#10530));
#10532=SURFACE_STYLE_USAGE(.BOTH.,#10531);
#10533=PRESENTATION_STYLE_ASSIGNMENT((#10532));
#10534=COLOUR_RGB('Sky Blue',0.24,0.69,0.87);
#10535=FILL_AREA_STYLE_COLOUR('',#10534);
#10536=FILL_AREA_STYLE('',(#10535));
#10537=SURFACE_STYLE_FILL_AREA(#10536);
#10538=SURFACE_SIDE_STYLE('',(#10537));
#10539=SURFACE_STYLE_USAGE(.BOTH.,#10538);
#10540=PRESENTATION_STYLE_ASSIGNMENT((#10539));
#10541=COLOUR_RGB('Grey',0.48,0.52,0.57);
#10542=FILL_AREA_STYLE_COLOUR('',#10541);
#10543=FILL_AREA_STYLE('',(#10542));
#10544=SURFACE_STYLE_FILL_AREA(#10543);
#10545=SURFACE_SIDE_STYLE('',(#10544));
#10546=SURFACE_STYLE_USAGE(.BOTH.,#10545);
#10547=PRESENTATION_STYLE_ASSIGNMENT((#10546));
#10548=COLOUR_RGB('Black',0.12,0.14,0.17);
#10549=FILL_AREA_STYLE_COLOUR('',#10548);
#10550=FILL_AREA_STYLE('',(#10549));
#10551=SURFACE_STYLE_FILL_AREA(#10550);
#10552=SURFACE_SIDE_STYLE('',(#10551));
#10553=SURFACE_STYLE_USAGE(.BOTH.,#10552);
#10554=PRESENTATION_STYLE_ASSIGNMENT((#10553));
#10555=COLOUR_RGB('Off White',0.89,0.88,0.83);
#10556=FILL_AREA_STYLE_COLOUR('',#10555);
#10557=FILL_AREA_STYLE('',(#10556));
#10558=SURFACE_STYLE_FILL_AREA(#10557);
#10559=SURFACE_SIDE_STYLE('',(#10558));
#10560=SURFACE_STYLE_USAGE(.BOTH.,#10559);
#10561=PRESENTATION_STYLE_ASSIGNMENT((#10560));
ENDSEC;
END-ISO-10303-21;
